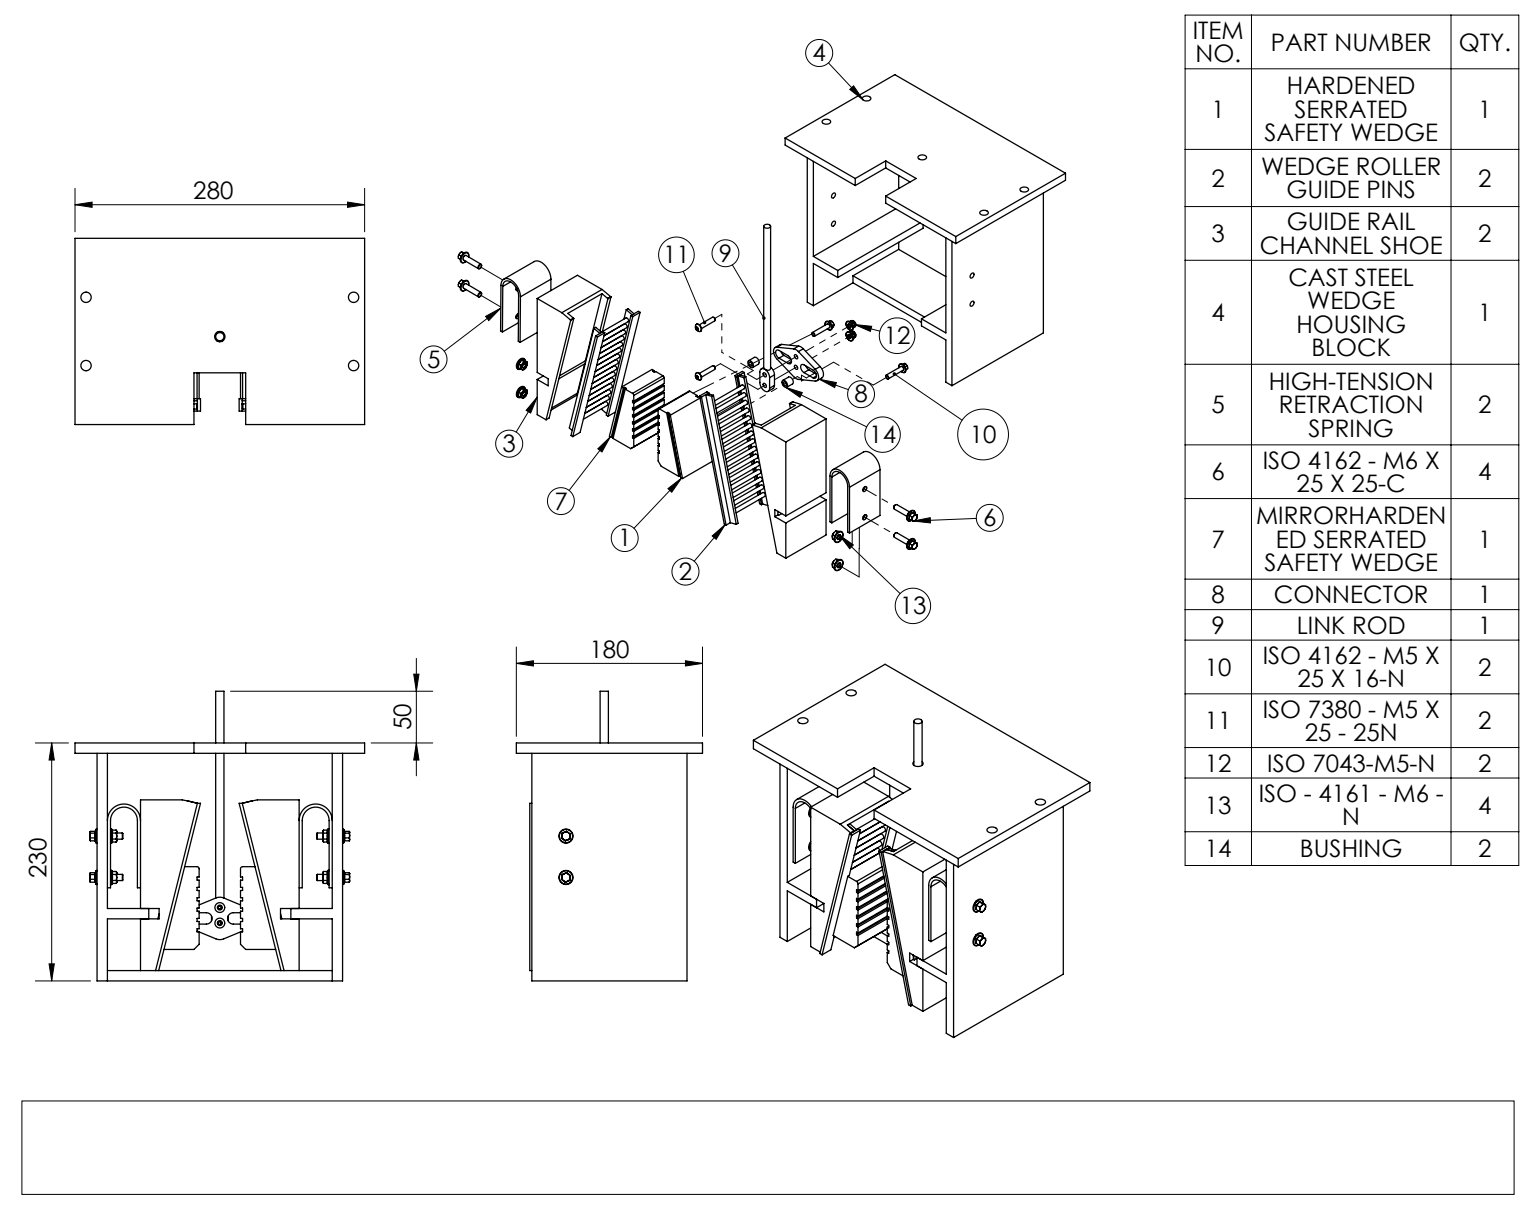
ISO-10303-21;
HEADER;
FILE_DESCRIPTION (('STEP AP214'),
    '1' );
FILE_NAME ('BR-599',
    '2026-09-24T10:26:00',
    ( '' ),
    ( '' ),
    'SwSTEP 2.0',
    'SolidWorks 2026',
    '' );
FILE_SCHEMA (( 'AUTOMOTIVE_DESIGN' ));
ENDSEC;

DATA;
#1 = VERTEX_POINT ( 'NONE', #3163 ) ;
#2 = DIRECTION ( 'NONE',  ( -1.000000000000000000, 0.000000000000000000, 0.000000000000000000 ) ) ;
#3 = CARTESIAN_POINT ( 'NONE',  ( 34.85300976710104948, 100.8957249956400375, 25.00000000000000000 ) ) ;
#4 = FACE_OUTER_BOUND ( 'NONE', #1590, .T. ) ;
#5 = CARTESIAN_POINT ( 'NONE',  ( -13.00000000000000533, 35.49999999999997158, 8.000000000000007105 ) ) ;
#6 = CIRCLE ( 'NONE', #8168, 300.0000000000001137 ) ;
#7 = CARTESIAN_POINT ( 'NONE',  ( 59.10657227073432551, 3.881474981106830313, 25.00000000000000000 ) ) ;
#8 = DIRECTION ( 'NONE',  ( 1.000000000000000000, 0.000000000000000000, 0.000000000000000000 ) ) ;
#9 = CARTESIAN_POINT ( 'NONE',  ( -4.101948962585905356, 2.368261337751086604, -3.381124513963614575 ) ) ;
#10 = ORIENTED_EDGE ( 'NONE', *, *, #2223, .T. ) ;
#11 = CARTESIAN_POINT ( 'NONE',  ( 36.99999999999999289, 80.00000000000000000, -25.00000000000000000 ) ) ;
#12 = DIRECTION ( 'NONE',  ( -1.000000000000000000, 0.000000000000000000, 0.000000000000000000 ) ) ;
#13 = DIRECTION ( 'NONE',  ( 0.000000000000000000, 4.440892098500621231E-16, 1.000000000000000000 ) ) ;
#14 = AXIS2_PLACEMENT_3D ( 'NONE', #9418, #3869, #11768 ) ;
#15 = VECTOR ( 'NONE', #13017, 1000.000000000000114 ) ;
#16 = LINE ( 'NONE', #8451, #3074 ) ;
#17 = EDGE_CURVE ( 'NONE', #13288, #10667, #2123, .T. ) ;
#18 = DIRECTION ( 'NONE',  ( 0.000000000000000000, -1.000000000000000000, 0.000000000000000000 ) ) ;
#19 = DIRECTION ( 'NONE',  ( -0.2425356250363330801, 0.9701425001453319874, 0.000000000000000000 ) ) ;
#20 = DIRECTION ( 'NONE',  ( -1.000000000000000000, 0.000000000000000000, 0.000000000000000000 ) ) ;
#21 = AXIS2_PLACEMENT_3D ( 'NONE', #11051, #3233, #13332 ) ;
#22 = CARTESIAN_POINT ( 'NONE',  ( 0.000000000000000000, 25.49999999999996803, 8.000000000000007105 ) ) ;
#23 = ORIENTED_EDGE ( 'NONE', *, *, #4123, .F. ) ;
#24 = COLOUR_RGB ( '', 0.66274510, 0.83137255, 0.94901961) ;
#25 = VERTEX_POINT ( 'NONE', #5412 ) ;
#26 = LINE ( 'NONE', #9828, #8340 ) ;
#27 = CONICAL_SURFACE ( 'NONE', #253, 2.540000000000002700, 0.7853981633974502774 ) ;
#28 = FILL_AREA_STYLE ('',( #13572 ) ) ;
#29 = VERTEX_POINT ( 'NONE', #870 ) ;
#30 = ADVANCED_FACE ( 'NONE', ( #11114 ), #7526, .T. ) ;
#31 = CARTESIAN_POINT ( 'NONE',  ( 0.1217565302851067177, -3.710888496608912845, 0.5725525826504656024 ) ) ;
#32 = VERTEX_POINT ( 'NONE', #2048 ) ;
#33 = ORIENTED_EDGE ( 'NONE', *, *, #5062, .T. ) ;
#34 = CONICAL_SURFACE ( 'NONE', #739, 4.000000000000004441, 1.047197551196600296 ) ;
#35 = VECTOR ( 'NONE', #3157, 1000.000000000000000 ) ;
#36 = VERTEX_POINT ( 'NONE', #7746 ) ;
#37 = EDGE_CURVE ( 'NONE', #1523, #9034, #1990, .T. ) ;
#38 = CARTESIAN_POINT ( 'NONE',  ( 3.903127820947815962E-15, 5.773502691896270633, -0.5999999999999894307 ) ) ;
#39 = LINE ( 'NONE', #7923, #9383 ) ;
#40 = CARTESIAN_POINT ( 'NONE',  ( 4.086376042167607636, -4.082715877136871008, 0.07147133206917684334 ) ) ;
#41 = CARTESIAN_POINT ( 'NONE',  ( -2.682243648011666259, -3.070208061305319536, -0.04852650426602220929 ) ) ;
#42 =( NAMED_UNIT ( * ) SI_UNIT ( $, .STERADIAN. ) SOLID_ANGLE_UNIT ( ) );
#43 = DIRECTION ( 'NONE',  ( 0.000000000000000000, 1.000000000000000000, 0.000000000000000000 ) ) ;
#44 = CARTESIAN_POINT ( 'NONE',  ( 4.050823680195247078, 3.779313952391380127, -0.5899027668435176119 ) ) ;
#45 = VERTEX_POINT ( 'NONE', #1089 ) ;
#46 = FILL_AREA_STYLE ('',( #8750 ) ) ;
#47 = VERTEX_POINT ( 'NONE', #6364 ) ;
#48 = AXIS2_PLACEMENT_3D ( 'NONE', #14299, #4291, #8725 ) ;
#49 = CARTESIAN_POINT ( 'NONE',  ( -129.3408537872145132, 199.5765550933606107, -75.00000000000001421 ) ) ;
#50 = CIRCLE ( 'NONE', #10087, 2.500000000000002220 ) ;
#51 = CIRCLE ( 'NONE', #7981, 2.500000000000002220 ) ;
#52 = DIRECTION ( 'NONE',  ( 0.000000000000000000, 0.000000000000000000, -1.000000000000000000 ) ) ;
#53 = EDGE_CURVE ( 'NONE', #1573, #2995, #7662, .T. ) ;
#54 = ORIENTED_EDGE ( 'NONE', *, *, #9609, .T. ) ;
#55 = VERTEX_POINT ( 'NONE', #5546 ) ;
#56 = ORIENTED_EDGE ( 'NONE', *, *, #8567, .F. ) ;
#57 = DIRECTION ( 'NONE',  ( 0.000000000000000000, 0.000000000000000000, -1.000000000000000000 ) ) ;
#58 = EDGE_CURVE ( 'NONE', #2255, #14288, #3932, .T. ) ;
#59 = MECHANICAL_DESIGN_GEOMETRIC_PRESENTATION_REPRESENTATION (  '', ( #3339 ), #8217 ) ;
#60 = ORIENTED_EDGE ( 'NONE', *, *, #8052, .T. ) ;
#61 = CARTESIAN_POINT ( 'NONE',  ( 0.000000000000000000, -0.8660254037844428154, 1.500000000000001332 ) ) ;
#62 = CIRCLE ( 'NONE', #4962, 5.000000000000000888 ) ;
#63 = PRODUCT ( 'bushing', 'bushing', '', ( #1978 ) ) ;
#64 = CARTESIAN_POINT ( 'NONE',  ( 0.000000000000000000, 0.000000000000000000, 0.000000000000000000 ) ) ;
#65 = CARTESIAN_POINT ( 'NONE',  ( 0.000000000000000000, 0.000000000000000000, -3.699999999999981082 ) ) ;
#66 = LINE ( 'NONE', #136, #7181 ) ;
#67 = B_SPLINE_CURVE_WITH_KNOTS ( 'NONE', 3,
 ( #11560, #3741, #1534, #5910, #10391, #8105 ),
 .UNSPECIFIED., .F., .F.,
 ( 4, 2, 4 ),
 ( 0.002365888236227980772, 0.003551327329835084114, 0.004736766423442187457 ),
 .UNSPECIFIED. ) ;
#68 = DIRECTION ( 'NONE',  ( -1.000000000000000000, 0.000000000000000000, 0.000000000000000000 ) ) ;
#69 = CARTESIAN_POINT ( 'NONE',  ( 22.00000000000000355, 30.00000000000000711, -25.00000000000000000 ) ) ;
#70 = LINE ( 'NONE', #7950, #11481 ) ;
#71 = MECHANICAL_DESIGN_GEOMETRIC_PRESENTATION_REPRESENTATION (  '', ( #7530 ), #1232 ) ;
#72 = EDGE_CURVE ( 'NONE', #4842, #5455, #11044, .T. ) ;
#73 = VERTEX_POINT ( 'NONE', #1987 ) ;
#74 = AXIS2_PLACEMENT_3D ( 'NONE', #8274, #12524, #8346 ) ;
#75 = EDGE_CURVE ( 'NONE', #7740, #14384, #13409, .T. ) ;
#76 = CARTESIAN_POINT ( 'NONE',  ( 4.142654963991838635, -2.035398498734361183, 3.525413613457314188 ) ) ;
#77 = AXIS2_PLACEMENT_3D ( 'NONE', #6500, #5341, #2338 ) ;
#78 = ORIENTED_EDGE ( 'NONE', *, *, #9945, .T. ) ;
#79 = VERTEX_POINT ( 'NONE', #5274 ) ;
#80 = CARTESIAN_POINT ( 'NONE',  ( 2.750000000000003997, 40.49999999999999289, 8.000000000000007105 ) ) ;
#81 = ORIENTED_EDGE ( 'NONE', *, *, #3321, .F. ) ;
#82 = CARTESIAN_POINT ( 'NONE',  ( -108.6817075744281595, 69.57655509336026967, 0.000000000000000000 ) ) ;
#83 = CARTESIAN_POINT ( 'NONE',  ( -5.000000000000000000, 0.9888715124523217437, -0.07061148569344526116 ) ) ;
#84 = CARTESIAN_POINT ( 'NONE',  ( -5.244935917792783897, 2.071347852254889155, -4.480280589322315876 ) ) ;
#85 = CARTESIAN_POINT ( 'NONE',  ( 2.855764796983339515, -2.970025579236438951, -0.09382832055446838071 ) ) ;
#86 = AXIS2_PLACEMENT_3D ( 'NONE', #5868, #6092, #4935 ) ;
#87 = EDGE_LOOP ( 'NONE', ( #13526, #11711, #10761, #2317 ) ) ;
#88 = FACE_OUTER_BOUND ( 'NONE', #2247, .T. ) ;
#89 = LINE ( 'NONE', #9889, #12206 ) ;
#90 = SURFACE_STYLE_FILL_AREA ( #4690 ) ;
#91 = DIRECTION ( 'NONE',  ( -0.000000000000000000, -0.000000000000000000, -1.000000000000000000 ) ) ;
#92 = ORIENTED_EDGE ( 'NONE', *, *, #1429, .T. ) ;
#93 = AXIS2_PLACEMENT_3D ( 'NONE', #10441, #13974, #10675 ) ;
#94 = CARTESIAN_POINT ( 'NONE',  ( -2.000000000000003997, 3.464101615137761492, -2.842992957459211212 ) ) ;
#95 = ADVANCED_FACE ( 'NONE', ( #9801 ), #3380, .T. ) ;
#96 = ADVANCED_FACE ( 'NONE', ( #3591 ), #13623, .F. ) ;
#97 = LINE ( 'NONE', #11278, #533 ) ;
#98 = DIRECTION ( 'NONE',  ( 0.000000000000000000, -1.000000000000000000, 0.000000000000000000 ) ) ;
#99 = PRODUCT_DEFINITION_SHAPE ( 'NONE', 'NONE',  #14480 ) ;
#100 = ORIENTED_EDGE ( 'NONE', *, *, #751, .T. ) ;
#101 = DIRECTION ( 'NONE',  ( 0.000000000000000000, 0.000000000000000000, -1.000000000000000000 ) ) ;
#102 = LINE ( 'NONE', #4701, #4263 ) ;
#103 = CARTESIAN_POINT ( 'NONE',  ( 0.000000000000000000, 0.000000000000000000, 1.599999999999990319 ) ) ;
#104 = CARTESIAN_POINT ( 'NONE',  ( 4.942471129496375681, -1.621204395475712046, 4.000000000000003553 ) ) ;
#105 = ORIENTED_EDGE ( 'NONE', *, *, #7029, .T. ) ;
#106 = LINE ( 'NONE', #11351, #1126 ) ;
#107 = EDGE_CURVE ( 'NONE', #8048, #4572, #11469, .T. ) ;
#108 =( NAMED_UNIT ( * ) PLANE_ANGLE_UNIT ( ) SI_UNIT ( $, .RADIAN. ) );
#109 = EDGE_CURVE ( 'NONE', #144, #5025, #8095, .T. ) ;
#110 = ORIENTED_EDGE ( 'NONE', *, *, #1310, .T. ) ;
#111 = CARTESIAN_POINT ( 'NONE',  ( 5.551115123125782702E-14, 3.464101615137764156, 2.000000000000001776 ) ) ;
#112 = ORIENTED_EDGE ( 'NONE', *, *, #12518, .T. ) ;
#113 = DIRECTION ( 'NONE',  ( 1.000000000000000000, 0.000000000000000000, -0.000000000000000000 ) ) ;
#114 = CYLINDRICAL_SURFACE ( 'NONE', #8701, 2.500000000000002220 ) ;
#115 = LINE ( 'NONE', #14321, #13122 ) ;
#116 = DIRECTION ( 'NONE',  ( 1.000000000000000000, 0.000000000000000000, 0.000000000000000000 ) ) ;
#117 = DIRECTION ( 'NONE',  ( -2.273843122241288438E-18, -5.551115123125783935E-17, -1.000000000000000000 ) ) ;
#118 = EDGE_CURVE ( 'NONE', #4637, #7467, #9051, .T. ) ;
#119 = CARTESIAN_POINT ( 'NONE',  ( 4.071447262713911996, -2.020725942163681399, 3.499999999999989342 ) ) ;
#120 = CARTESIAN_POINT ( 'NONE',  ( 22.00000000000000355, 30.00000000000000711, -25.00000000000000000 ) ) ;
#121 = ORIENTED_EDGE ( 'NONE', *, *, #9321, .T. ) ;
#122 = DIRECTION ( 'NONE',  ( -0.000000000000000000, -1.000000000000000000, -0.000000000000000000 ) ) ;
#123 = ADVANCED_FACE ( 'NONE', ( #3728 ), #1486, .F. ) ;
#124 = DIRECTION ( 'NONE',  ( -1.000000000000000000, -1.224646799147353454E-16, 0.000000000000000000 ) ) ;
#125 = EDGE_CURVE ( 'NONE', #5215, #588, #8984, .T. ) ;
#126 = ORIENTED_EDGE ( 'NONE', *, *, #8617, .F. ) ;
#127 = ORIENTED_EDGE ( 'NONE', *, *, #5175, .F. ) ;
#128 = ORIENTED_EDGE ( 'NONE', *, *, #2234, .F. ) ;
#129 = FACE_OUTER_BOUND ( 'NONE', #6696, .T. ) ;
#130 = EDGE_CURVE ( 'NONE', #3893, #6812, #6927, .T. ) ;
#131 = VERTEX_POINT ( 'NONE', #10090 ) ;
#132 = DIRECTION ( 'NONE',  ( -1.000000000000000000, -3.286707217423839940E-17, -2.273843122241288053E-18 ) ) ;
#133 = DIRECTION ( 'NONE',  ( -1.000000000000000000, 2.551526159633733968E-19, 1.987661601597216239E-18 ) ) ;
#134 = DIRECTION ( 'NONE',  ( 0.000000000000000000, 0.000000000000000000, 1.000000000000000000 ) ) ;
#135 = ADVANCED_FACE ( 'NONE', ( #12436 ), #6529, .F. ) ;
#136 = CARTESIAN_POINT ( 'NONE',  ( 19.99999999999999645, 67.00000000000000000, -25.00000000000000000 ) ) ;
#137 = CARTESIAN_POINT ( 'NONE',  ( 3.000000000000000888, 3.469446951953614189E-15, -25.03750572909319061 ) ) ;
#138 = AXIS2_PLACEMENT_3D ( 'NONE', #9240, #11510, #4853 ) ;
#139 = FACE_OUTER_BOUND ( 'NONE', #10085, .T. ) ;
#140 = DIRECTION ( 'NONE',  ( 0.000000000000000000, 1.000000000000000000, 0.000000000000000000 ) ) ;
#141 = EDGE_CURVE ( 'NONE', #4176, #9400, #11330, .T. ) ;
#142 = CARTESIAN_POINT ( 'NONE',  ( 5.085009042717538286, 2.271170964606955778, 4.066216496625539634 ) ) ;
#143 = ORIENTED_EDGE ( 'NONE', *, *, #10591, .T. ) ;
#144 = VERTEX_POINT ( 'NONE', #80 ) ;
#145 = CARTESIAN_POINT ( 'NONE',  ( -2.712778981739159878, 3.052578478157618846, -3.130620751972420734 ) ) ;
#146 = ORIENTED_EDGE ( 'NONE', *, *, #7792, .F. ) ;
#147 = EDGE_LOOP ( 'NONE', ( #10800, #705, #1394, #14407 ) ) ;
#148 = CARTESIAN_POINT ( 'NONE',  ( 0.8653900595644522520, -5.556556492855608376, -4.490801088233122407 ) ) ;
#149 = LINE ( 'NONE', #2412, #13592 ) ;
#150 = EDGE_CURVE ( 'NONE', #7089, #2949, #9184, .T. ) ;
#151 = CARTESIAN_POINT ( 'NONE',  ( 2.171643655288374664, -3.365003104552342972, -1.643201566025979943E-14 ) ) ;
#152 = CARTESIAN_POINT ( 'NONE',  ( 6.800000000000028244, -4.618802153517003184, 0.000000000000000000 ) ) ;
#153 = FACE_OUTER_BOUND ( 'NONE', #11102, .T. ) ;
#154 = CARTESIAN_POINT ( 'NONE',  ( 58.68170757442803165, 29.57655509336062849, -33.00000000000000000 ) ) ;
#155 = ORIENTED_EDGE ( 'NONE', *, *, #6137, .F. ) ;
#156 = CARTESIAN_POINT ( 'NONE',  ( 0.2484800633749933707, -4.430380094434230642, -0.3263565795981031581 ) ) ;
#157 = AXIS2_PLACEMENT_3D ( 'NONE', #14374, #7610, #12245 ) ;
#158 = ORIENTED_EDGE ( 'NONE', *, *, #2244, .F. ) ;
#159 = CARTESIAN_POINT ( 'NONE',  ( 56.68121602037099649, 13.58289998256015352, 25.00000000000000000 ) ) ;
#160 = LINE ( 'NONE', #229, #1194 ) ;
#161 = EDGE_CURVE ( 'NONE', #1060, #1016, #5743, .T. ) ;
#162 = DIRECTION ( 'NONE',  ( 0.000000000000000000, -1.000000000000000000, 0.000000000000000000 ) ) ;
#163 = EDGE_CURVE ( 'NONE', #6145, #1954, #4682, .T. ) ;
#164 = ORIENTED_EDGE ( 'NONE', *, *, #6756, .F. ) ;
#165 = DIRECTION ( 'NONE',  ( 1.734723475976770502E-18, -4.440892098500621231E-16, -1.000000000000000000 ) ) ;
#166 = VECTOR ( 'NONE', #2081, 1000.000000000000000 ) ;
#167 = CARTESIAN_POINT ( 'NONE',  ( 0.000000000000000000, 0.000000000000000000, 0.000000000000000000 ) ) ;
#168 = CONICAL_SURFACE ( 'NONE', #12822, 1732.050807568857181, 1.047197551196592746 ) ;
#169 = ORIENTED_EDGE ( 'NONE', *, *, #8329, .T. ) ;
#170 = CARTESIAN_POINT ( 'NONE',  ( 59.91362529070399034, 29.57655509336063560, -28.00000000000000000 ) ) ;
#171 = PRODUCT_DEFINITION_SHAPE ( 'NONE', 'NONE',  #7761 ) ;
#172 = VERTEX_POINT ( 'NONE', #3659 ) ;
#173 = FACE_OUTER_BOUND ( 'NONE', #6648, .T. ) ;
#174 = LINE ( 'NONE', #1203, #523 ) ;
#175 = AXIS2_PLACEMENT_3D ( 'NONE', #2230, #7697, #10922 ) ;
#176 = AXIS2_PLACEMENT_3D ( 'NONE', #8540, #7429, #5033 ) ;
#177 = DIRECTION ( 'NONE',  ( 0.000000000000000000, 0.000000000000000000, -1.000000000000000000 ) ) ;
#178 = LINE ( 'NONE', #1338, #11397 ) ;
#179 =( NAMED_UNIT ( * ) PLANE_ANGLE_UNIT ( ) SI_UNIT ( $, .RADIAN. ) );
#180 = LINE ( 'NONE', #12266, #3484 ) ;
#181 = VERTEX_POINT ( 'NONE', #10380 ) ;
#182 = CARTESIAN_POINT ( 'NONE',  ( 0.000000000000000000, 0.000000000000000000, 0.000000000000000000 ) ) ;
#183 = ORIENTED_EDGE ( 'NONE', *, *, #4806, .T. ) ;
#184 = DIRECTION ( 'NONE',  ( -1.000000000000000000, 0.000000000000000000, 0.000000000000000000 ) ) ;
#185 = ORIENTED_EDGE ( 'NONE', *, *, #3525, .T. ) ;
#186 = DIRECTION ( 'NONE',  ( 0.000000000000000000, 0.000000000000000000, -1.000000000000000000 ) ) ;
#187 = AXIS2_PLACEMENT_3D ( 'NONE', #14289, #6433, #6375 ) ;
#188 = AXIS2_PLACEMENT_3D ( 'NONE', #12778, #9636, #495 ) ;
#189 = EDGE_LOOP ( 'NONE', ( #816, #9707, #13523, #12144 ) ) ;
#190 = EDGE_LOOP ( 'NONE', ( #12989, #13833, #3490, #10771 ) ) ;
#191 = FACE_OUTER_BOUND ( 'NONE', #2606, .T. ) ;
#192 = VERTEX_POINT ( 'NONE', #361 ) ;
#193 = PLANE ( 'NONE',  #1641 ) ;
#194 = EDGE_CURVE ( 'NONE', #2847, #8895, #12600, .T. ) ;
#195 = ADVANCED_FACE ( 'NONE', ( #8392 ), #5103, .F. ) ;
#196 = AXIS2_PLACEMENT_3D ( 'NONE', #5459, #4385, #14329 ) ;
#197 = DIRECTION ( 'NONE',  ( -1.000000000000000000, -0.000000000000000000, -0.000000000000000000 ) ) ;
#198 = LINE ( 'NONE', #5806, #5338 ) ;
#199 = VECTOR ( 'NONE', #5956, 1000.000000000000000 ) ;
#200 = ITEM_DEFINED_TRANSFORMATION ( 'NONE', 'NONE', #5460,  #11025 ) ;
#201 = VECTOR ( 'NONE', #12349, 1000.000000000000000 ) ;
#202 = PLANE ( 'NONE',  #7722 ) ;
#203 = CARTESIAN_POINT ( 'NONE',  ( -4.204114099329524734, 1.660341531092956124, -3.302132361967865748 ) ) ;
#204 = CARTESIAN_POINT ( 'NONE',  ( 4.071447262713911996, 2.020725942163681399, -3.499999999999996003 ) ) ;
#205 = EDGE_CURVE ( 'NONE', #13026, #14419, #660, .T. ) ;
#206 = EDGE_CURVE ( 'NONE', #7155, #8446, #11531, .T. ) ;
#207 = ORIENTED_EDGE ( 'NONE', *, *, #6472, .T. ) ;
#208 = AXIS2_PLACEMENT_3D ( 'NONE', #12173, #7777, #14450 ) ;
#209 = ORIENTED_EDGE ( 'NONE', *, *, #6776, .T. ) ;
#210 = CARTESIAN_POINT ( 'NONE',  ( 22.00000000000000355, 40.00000000000000711, 25.00000000000000000 ) ) ;
#211 = ORIENTED_EDGE ( 'NONE', *, *, #12673, .T. ) ;
#212 = DIRECTION ( 'NONE',  ( 0.000000000000000000, 1.000000000000000000, 0.000000000000000000 ) ) ;
#213 = EDGE_CURVE ( 'NONE', #6553, #4911, #14362, .T. ) ;
#214 = CARTESIAN_POINT ( 'NONE',  ( 8.000000000000000000, 25.49999999999996803, 8.000000000000007105 ) ) ;
#215 = LINE ( 'NONE', #3596, #1161 ) ;
#216 = CARTESIAN_POINT ( 'NONE',  ( 0.1391502195351374815, -4.241015250120806712, 0.6543461111163237920 ) ) ;
#217 = CARTESIAN_POINT ( 'NONE',  ( 56.75585977000769589, 23.28432498401347672, 25.00000000000000000 ) ) ;
#218 = DIRECTION ( 'NONE',  ( 0.000000000000000000, 0.000000000000000000, 1.000000000000000000 ) ) ;
#219 = CARTESIAN_POINT ( 'NONE',  ( 62.10586122665984732, -20.42344490663941414, -23.00000000000000000 ) ) ;
#220 = EDGE_LOOP ( 'NONE', ( #2917, #1884 ) ) ;
#221 = AXIS2_PLACEMENT_3D ( 'NONE', #6634, #1226, #3433 ) ;
#222 = DIRECTION ( 'NONE',  ( 1.000000000000000000, 0.000000000000000000, 0.000000000000000000 ) ) ;
#223 = VECTOR ( 'NONE', #6277, 1000.000000000000000 ) ;
#224 = ORIENTED_EDGE ( 'NONE', *, *, #11005, .F. ) ;
#225 = EDGE_CURVE ( 'NONE', #10568, #2459, #4887, .T. ) ;
#226 = ORIENTED_EDGE ( 'NONE', *, *, #6230, .T. ) ;
#227 = AXIS2_PLACEMENT_3D ( 'NONE', #3286, #6852, #12205 ) ;
#228 = CARTESIAN_POINT ( 'NONE',  ( 22.00000000000000000, 67.00000000000000000, 25.00000000000000000 ) ) ;
#229 = CARTESIAN_POINT ( 'NONE',  ( 24.99999999999999289, -4.898587196589414604E-15, -25.00000000000000000 ) ) ;
#230 = EDGE_CURVE ( 'NONE', #2483, #11506, #8245, .T. ) ;
#231 = FILL_AREA_STYLE_COLOUR ( '', #8450 ) ;
#232 = B_SPLINE_CURVE_WITH_KNOTS ( 'NONE', 3,
 ( #9885, #3384, #13193, #4342, #3307, #6720, #12149, #7750, #12227, #4273 ),
 .UNSPECIFIED., .F., .F.,
 ( 4, 2, 2, 2, 4 ),
 ( 0.000000000000000000, 0.001528561485809837566, 0.003057122971619675132, 0.004585684457429512265, 0.006114245943239350264 ),
 .UNSPECIFIED. ) ;
#233 = ORIENTED_EDGE ( 'NONE', *, *, #8707, .F. ) ;
#234 = ORIENTED_EDGE ( 'NONE', *, *, #1565, .T. ) ;
#235 = CARTESIAN_POINT ( 'NONE',  ( 0.000000000000000000, 25.49999999999996803, 8.000000000000007105 ) ) ;
#236 = DIRECTION ( 'NONE',  ( 1.000000000000000000, -0.000000000000000000, -0.000000000000000000 ) ) ;
#237 = AXIS2_PLACEMENT_3D ( 'NONE', #9091, #4649, #3762 ) ;
#238 = ORIENTED_EDGE ( 'NONE', *, *, #350, .F. ) ;
#239 = EDGE_CURVE ( 'NONE', #9259, #13438, #9577, .T. ) ;
#240 = CARTESIAN_POINT ( 'NONE',  ( -5.184911785341042467, -2.993510214990505514, -4.630720594357042863 ) ) ;
#241 = EDGE_CURVE ( 'NONE', #3192, #10542, #6150, .T. ) ;
#242 = CARTESIAN_POINT ( 'NONE',  ( 4.000000000000003553, 2.309401076758501592, -4.699999999999981526 ) ) ;
#243 = DIRECTION ( 'NONE',  ( 1.000000000000000000, 1.723842398015259277E-15, 0.000000000000000000 ) ) ;
#244 = B_SPLINE_CURVE_WITH_KNOTS ( 'NONE', 3,
 ( #6085, #473, #399, #10567, #328 ),
 .UNSPECIFIED., .F., .F.,
 ( 4, 1, 4 ),
 ( 0.000000000000000000, 0.002309401076758502321, 0.004618802153517004641 ),
 .UNSPECIFIED. ) ;
#245 = ORIENTED_EDGE ( 'NONE', *, *, #3357, .T. ) ;
#246 = AXIS2_PLACEMENT_3D ( 'NONE', #2195, #9875, #11107 ) ;
#247 = CARTESIAN_POINT ( 'NONE',  ( 4.175326769692832229, -2.060699556488890138, -3.569236330973504678 ) ) ;
#248 = CIRCLE ( 'NONE', #2365, 2.500000000000000444 ) ;
#249 = DIRECTION ( 'NONE',  ( 1.000000000000000000, -2.551526159633733968E-19, -1.987661601597216239E-18 ) ) ;
#250 = PRESENTATION_STYLE_ASSIGNMENT (( #7854 ) ) ;
#251 = DIRECTION ( 'NONE',  ( 2.732679788978641511E-17, 0.8660254037844375974, -0.5000000000000019984 ) ) ;
#252 = LINE ( 'NONE', #13664, #5773 ) ;
#253 = AXIS2_PLACEMENT_3D ( 'NONE', #8429, #2964, #14156 ) ;
#254 = VERTEX_POINT ( 'NONE', #10524 ) ;
#255 = DIRECTION ( 'NONE',  ( 0.000000000000000000, 0.000000000000000000, 1.000000000000000000 ) ) ;
#256 = ORIENTED_EDGE ( 'NONE', *, *, #409, .F. ) ;
#257 = FACE_OUTER_BOUND ( 'NONE', #7644, .T. ) ;
#258 = VECTOR ( 'NONE', #7960, 1000.000000000000000 ) ;
#259 = FACE_OUTER_BOUND ( 'NONE', #5577, .T. ) ;
#260 = VERTEX_POINT ( 'NONE', #11845 ) ;
#261 = LINE ( 'NONE', #9100, #14213 ) ;
#262 = VECTOR ( 'NONE', #2943, 1000.000000000000114 ) ;
#263 = AXIS2_PLACEMENT_3D ( 'NONE', #12477, #3770, #2452 ) ;
#264 = ADVANCED_FACE ( 'NONE', ( #14056 ), #3951, .T. ) ;
#265 = EDGE_LOOP ( 'NONE', ( #8330, #2797, #508, #8925 ) ) ;
#266 = ORIENTED_EDGE ( 'NONE', *, *, #8071, .F. ) ;
#267 = ORIENTED_EDGE ( 'NONE', *, *, #8811, .F. ) ;
#268 = CIRCLE ( 'NONE', #9369, 5.000000000000004441 ) ;
#269 = VERTEX_POINT ( 'NONE', #12870 ) ;
#270 = DIRECTION ( 'NONE',  ( 0.000000000000000000, -8.482162385747133845E-47, 1.000000000000000000 ) ) ;
#271 = CARTESIAN_POINT ( 'NONE',  ( 66.53192852109765454, -5.819950020346492892, -25.00000000000000000 ) ) ;
#272 = ORIENTED_EDGE ( 'NONE', *, *, #3606, .T. ) ;
#273 = FACE_OUTER_BOUND ( 'NONE', #4402, .T. ) ;
#274 = CARTESIAN_POINT ( 'NONE',  ( 5.253687138749954855, 3.069401043531180484, -4.666239469495483405 ) ) ;
#275 = FILL_AREA_STYLE_COLOUR ( '', #447 ) ;
#276 = DIRECTION ( 'NONE',  ( 0.000000000000000000, 0.000000000000000000, 1.000000000000000000 ) ) ;
#277 = PRESENTATION_LAYER_ASSIGNMENT (  '', '', ( #3555 ) ) ;
#278 = VECTOR ( 'NONE', #5827, 1000.000000000000227 ) ;
#279 = CARTESIAN_POINT ( 'NONE',  ( 0.2174200650117580069, 3.876582599186215727, 0.2855619784720741516 ) ) ;
#280 = CYLINDRICAL_SURFACE ( 'NONE', #1408, 2.500000000000002220 ) ;
#281 = FACE_OUTER_BOUND ( 'NONE', #2970, .T. ) ;
#282 = CARTESIAN_POINT ( 'NONE',  ( 5.000000000000001776, -0.9835753746177059442, -0.05800540215398873600 ) ) ;
#283 = EDGE_CURVE ( 'NONE', #3285, #4147, #432, .T. ) ;
#284 = VECTOR ( 'NONE', #9089, 1000.000000000000000 ) ;
#285 = COLOUR_RGB ( '', 0.40784314, 0.44705882, 0.49803922) ;
#286 = ORIENTED_EDGE ( 'NONE', *, *, #14219, .T. ) ;
#287 = AXIS2_PLACEMENT_3D ( 'NONE', #9499, #13966, #10597 ) ;
#288 = VECTOR ( 'NONE', #14234, 1000.000000000000000 ) ;
#289 = ORIENTED_EDGE ( 'NONE', *, *, #2632, .T. ) ;
#290 = DIRECTION ( 'NONE',  ( -1.000000000000000000, 0.000000000000000000, 0.000000000000000000 ) ) ;
#291 = ORIENTED_EDGE ( 'NONE', *, *, #5105, .F. ) ;
#292 = ORIENTED_EDGE ( 'NONE', *, *, #11801, .F. ) ;
#293 = EDGE_CURVE ( 'NONE', #3067, #10101, #2628, .T. ) ;
#294 = FACE_OUTER_BOUND ( 'NONE', #7069, .T. ) ;
#295 = DIRECTION ( 'NONE',  ( -1.000000000000000000, -1.665334536937734318E-16, 0.000000000000000000 ) ) ;
#296 = CARTESIAN_POINT ( 'NONE',  ( 61.53192852109764743, -5.819950020346492892, -25.00000000000000000 ) ) ;
#297 = CARTESIAN_POINT ( 'NONE',  ( 28.00000000000000355, 29.99999999999999645, -6.999999999999992006 ) ) ;
#298 = PLANE ( 'NONE',  #9372 ) ;
#299 = EDGE_CURVE ( 'NONE', #11445, #8749, #1752, .T. ) ;
#300 = DIRECTION ( 'NONE',  ( -1.000000000000000000, -1.276920294826118092E-16, 0.000000000000000000 ) ) ;
#301 = VECTOR ( 'NONE', #2565, 1000.000000000000000 ) ;
#302 = AXIS2_PLACEMENT_3D ( 'NONE', #9953, #7666, #5414 ) ;
#303 = PRODUCT_DEFINITION_SHAPE ( 'NONE', 'NONE',  #14478 ) ;
#304 = CARTESIAN_POINT ( 'NONE',  ( 63.34848382498275754, 15.83712095624566984, 0.000000000000000000 ) ) ;
#305 = EDGE_CURVE ( 'NONE', #1178, #14168, #3877, .T. ) ;
#306 = EDGE_LOOP ( 'NONE', ( #9617, #6629, #11279, #5233, #2336 ) ) ;
#307 = UNCERTAINTY_MEASURE_WITH_UNIT (LENGTH_MEASURE( 1.000000000000000082E-05 ), #6803, 'distance_accuracy_value', 'NONE');
#308 = AXIS2_PLACEMENT_3D ( 'NONE', #4405, #11111, #14418 ) ;
#309 = CARTESIAN_POINT ( 'NONE',  ( -4.177163563997808592E-15, -5.914770570062451327, -4.581776566113613391 ) ) ;
#310 = DIRECTION ( 'NONE',  ( -0.000000000000000000, -0.000000000000000000, -1.000000000000000000 ) ) ;
#311 = EDGE_CURVE ( 'NONE', #7235, #651, #5038, .T. ) ;
#312 = EDGE_CURVE ( 'NONE', #10181, #36, #9348, .T. ) ;
#313 = VERTEX_POINT ( 'NONE', #3807 ) ;
#314 = LINE ( 'NONE', #11495, #3240 ) ;
#315 = AXIS2_PLACEMENT_3D ( 'NONE', #13880, #3856, #13947 ) ;
#316 = CARTESIAN_POINT ( 'NONE',  ( 5.000882498481321825, 2.309401076758504257, -4.000000000000005329 ) ) ;
#317 = ORIENTED_EDGE ( 'NONE', *, *, #8785, .T. ) ;
#318 = DIRECTION ( 'NONE',  ( 0.000000000000000000, 0.000000000000000000, -1.000000000000000000 ) ) ;
#319 = AXIS2_PLACEMENT_3D ( 'NONE', #14262, #4250, #9862 ) ;
#320 = ORIENTED_EDGE ( 'NONE', *, *, #6806, .T. ) ;
#321 = CARTESIAN_POINT ( 'NONE',  ( -1.655952806101420816, 3.662737355149043417, -7.859618717572649691E-15 ) ) ;
#322 = CARTESIAN_POINT ( 'NONE',  ( 4.960798468789974436, -4.316040323963732384, 0.6738506825564457570 ) ) ;
#323 = CARTESIAN_POINT ( 'NONE',  ( 4.142654963991838635, -2.035398498734360739, -3.525413613457307083 ) ) ;
#324 = PLANE ( 'NONE',  #4421 ) ;
#325 = FILL_AREA_STYLE ('',( #4788 ) ) ;
#326 = CARTESIAN_POINT ( 'NONE',  ( 5.211749180171795892, 2.764497899775253398, -4.327903350935040194 ) ) ;
#327 = EDGE_CURVE ( 'NONE', #12296, #10667, #14351, .T. ) ;
#328 = CARTESIAN_POINT ( 'NONE',  ( 4.988724804725785944, -2.309401076758511806, -3.999999999999989786 ) ) ;
#329 = ORIENTED_EDGE ( 'NONE', *, *, #2055, .F. ) ;
#330 = FACE_OUTER_BOUND ( 'NONE', #10664, .T. ) ;
#331 = AXIS2_PLACEMENT_3D ( 'NONE', #13223, #14112, #7625 ) ;
#332 = EDGE_LOOP ( 'NONE', ( #2235, #9839 ) ) ;
#333 = CARTESIAN_POINT ( 'NONE',  ( 108.6817075744280174, -30.42344490663958112, 33.00000000000002842 ) ) ;
#334 = LINE ( 'NONE', #480, #12683 ) ;
#335 = ORIENTED_EDGE ( 'NONE', *, *, #3874, .F. ) ;
#336 = LINE ( 'NONE', #6016, #9990 ) ;
#337 = VERTEX_POINT ( 'NONE', #12933 ) ;
#338 = ORIENTED_EDGE ( 'NONE', *, *, #3386, .T. ) ;
#339 = DIRECTION ( 'NONE',  ( 1.000000000000000000, 0.000000000000000000, -0.000000000000000000 ) ) ;
#340 = EDGE_LOOP ( 'NONE', ( #2490, #1652, #2077 ) ) ;
#341 = CARTESIAN_POINT ( 'NONE',  ( 7.500000000000029310, 29.99999999999999289, 0.000000000000000000 ) ) ;
#342 = CYLINDRICAL_SURFACE ( 'NONE', #2622, 4.000000000000001776 ) ;
#343 = CLOSED_SHELL ( 'NONE', ( #348, #10277, #10610, #2946, #4930, #5603, #8583, #3122, #8964, #584, #2814, #2804, #5042, #11746, #8231, #7567, #9589, #9255, #10929, #2822, #4189, #8522, #2178, #12387, #5966, #9430, #5583, #8276, #5909 ) ) ;
#344 = ORIENTED_EDGE ( 'NONE', *, *, #679, .T. ) ;
#345 = DIRECTION ( 'NONE',  ( 0.000000000000000000, 0.000000000000000000, -1.000000000000000000 ) ) ;
#346 = CARTESIAN_POINT ( 'NONE',  ( 0.2484800633750008092, -2.497823135841239939, 3.673643420401929482 ) ) ;
#347 = PRESENTATION_STYLE_ASSIGNMENT (( #11533 ) ) ;
#348 = ADVANCED_FACE ( 'NONE', ( #1821 ), #11776, .T. ) ;
#349 = CARTESIAN_POINT ( 'NONE',  ( 5.599999999999994316, -4.041451884327377009, 0.000000000000000000 ) ) ;
#350 = EDGE_CURVE ( 'NONE', #1315, #10506, #376, .T. ) ;
#351 = DIRECTION ( 'NONE',  ( 0.000000000000000000, 0.000000000000000000, 1.000000000000000000 ) ) ;
#352 = CARTESIAN_POINT ( 'NONE',  ( 25.00000000000000000, 189.5765550933606107, 47.99999999999998579 ) ) ;
#353 = PLANE ( 'NONE',  #1336 ) ;
#354 = CARTESIAN_POINT ( 'NONE',  ( -2.749999999999997780, 25.49999999999996803, 8.000000000000007105 ) ) ;
#355 = CARTESIAN_POINT ( 'NONE',  ( 20.00000000000000000, 70.00000000000000000, 25.00000000000000000 ) ) ;
#356 = EDGE_CURVE ( 'NONE', #7502, #4025, #7084, .T. ) ;
#357 = ORIENTED_EDGE ( 'NONE', *, *, #6598, .T. ) ;
#358 = ORIENTED_EDGE ( 'NONE', *, *, #8649, .F. ) ;
#359 = EDGE_LOOP ( 'NONE', ( #6846, #13028, #8516, #4534 ) ) ;
#360 = AXIS2_PLACEMENT_3D ( 'NONE', #1411, #10345, #9164 ) ;
#361 = CARTESIAN_POINT ( 'NONE',  ( 35.00229726637439143, 120.2985749985466839, 25.00000000000000000 ) ) ;
#362 = ORIENTED_EDGE ( 'NONE', *, *, #4420, .T. ) ;
#363 = FACE_BOUND ( 'NONE', #5930, .T. ) ;
#364 = CARTESIAN_POINT ( 'NONE',  ( 5.122341571230623281, 2.957385285031203459, -4.581776566113601845 ) ) ;
#365 = CARTESIAN_POINT ( 'NONE',  ( 129.3408537872138595, 189.5765550933606107, -4.000000000000019540 ) ) ;
#366 = DIRECTION ( 'NONE',  ( 0.000000000000000000, 0.000000000000000000, 1.000000000000000000 ) ) ;
#367 = EDGE_CURVE ( 'NONE', #6880, #5464, #10123, .T. ) ;
#368 = CARTESIAN_POINT ( 'NONE',  ( 1.671902908347949033E-15, 2.686816014504571193, 2.346298152288376127 ) ) ;
#369 = DIRECTION ( 'NONE',  ( 1.000000000000000000, 0.000000000000000000, 0.000000000000000000 ) ) ;
#370 = ADVANCED_FACE ( 'NONE', ( #3209 ), #923, .F. ) ;
#371 = LINE ( 'NONE', #6940, #6098 ) ;
#372 = DIRECTION ( 'NONE',  ( -1.000000000000000000, 0.000000000000000000, 0.000000000000000000 ) ) ;
#373 = VERTEX_POINT ( 'NONE', #7643 ) ;
#374 = AXIS2_PLACEMENT_3D ( 'NONE', #6234, #5287, #14092 ) ;
#375 = VERTEX_POINT ( 'NONE', #14335 ) ;
#376 = B_SPLINE_CURVE_WITH_KNOTS ( 'NONE', 3,
 ( #7503, #2032, #11022, #6628, #11096, #11995 ),
 .UNSPECIFIED., .F., .F.,
 ( 4, 2, 4 ),
 ( 0.01308430721348208085, 0.01410661710602280003, 0.01512892699856351920 ),
 .UNSPECIFIED. ) ;
#377 = ADVANCED_FACE ( 'NONE', ( #4324 ), #12061, .F. ) ;
#378 = ORIENTED_EDGE ( 'NONE', *, *, #1938, .F. ) ;
#379 = CARTESIAN_POINT ( 'NONE',  ( 4.851472949720997185, 2.694301256218259777, -3.333333333333333925 ) ) ;
#380 = DIRECTION ( 'NONE',  ( 0.000000000000000000, 0.000000000000000000, -1.000000000000000000 ) ) ;
#381 = EDGE_CURVE ( 'NONE', #10071, #10068, #6343, .T. ) ;
#382 = EDGE_CURVE ( 'NONE', #1594, #11544, #7791, .T. ) ;
#383 = ORIENTED_EDGE ( 'NONE', *, *, #7969, .F. ) ;
#384 = EDGE_LOOP ( 'NONE', ( #8379, #6792, #7299, #1071, #1051 ) ) ;
#385 = CARTESIAN_POINT ( 'NONE',  ( 54.33050351964436686, 32.98574998546678927, 25.00000000000000000 ) ) ;
#386 = CARTESIAN_POINT ( 'NONE',  ( 5.076540720129295359, 2.330508241952946147, -4.036558682520523966 ) ) ;
#387 = ORIENTED_EDGE ( 'NONE', *, *, #10769, .T. ) ;
#388 =( BOUNDED_SURFACE ( )  B_SPLINE_SURFACE ( 3, 2, ( 
 ( #3636, #8070, #4659 ),
 ( #3858, #7047, #7120 ),
 ( #6973, #4862, #11444 ),
 ( #3572, #2599, #9324 ),
 ( #12766, #9250, #13809 ),
 ( #13596, #1568, #3776 ) ),
 .UNSPECIFIED., .F., .F., .T. ) 
 B_SPLINE_SURFACE_WITH_KNOTS ( ( 4, 2, 4 ),
 ( 3, 3 ),
 ( 0.01886032586153034776, 0.02121253401777977582, 0.02356474217402920734 ),
 ( 0.000000000000000000, 1.000000000000000000 ),
 .UNSPECIFIED. ) 
 GEOMETRIC_REPRESENTATION_ITEM ( )  RATIONAL_B_SPLINE_SURFACE ( (
 ( 1.000000000000000000, 0.8047781103519398016, 1.000000000000000000),
 ( 1.000000000000000000, 0.8123785825774555436, 1.000000000000000000),
 ( 1.000000000000000000, 0.8190671539561653614, 1.000000000000000000),
 ( 1.000000000000000000, 0.8192352255061488009, 1.000000000000000000),
 ( 1.000000000000000000, 0.8126129677041400434, 1.000000000000000000),
 ( 1.000000000000000000, 0.8047712537969720081, 1.000000000000000000) ) ) 
 REPRESENTATION_ITEM ( '' )  SURFACE ( )  );
#389 = CARTESIAN_POINT ( 'NONE',  ( 1.560000000000005826, 0.8660254037844428154, 1.500000000000001332 ) ) ;
#390 = EDGE_CURVE ( 'NONE', #9890, #13868, #13175, .T. ) ;
#391 = DIRECTION ( 'NONE',  ( 0.000000000000000000, -0.000000000000000000, 1.000000000000000000 ) ) ;
#392 = CARTESIAN_POINT ( 'NONE',  ( 4.082498951862935321, 2.020725942163681399, 3.499999999999996003 ) ) ;
#393 = ORIENTED_EDGE ( 'NONE', *, *, #4064, .F. ) ;
#394 = CARTESIAN_POINT ( 'NONE',  ( -5.244818697407745312, 2.029379090245553741, -4.490884354499010023 ) ) ;
#395 = DIRECTION ( 'NONE',  ( 1.000000000000000000, 3.916739600140467622E-15, 0.000000000000000000 ) ) ;
#396 = AXIS2_PLACEMENT_3D ( 'NONE', #2897, #625, #12994 ) ;
#397 = DIRECTION ( 'NONE',  ( 0.000000000000000000, 0.000000000000000000, -1.000000000000000000 ) ) ;
#398 = ORIENTED_EDGE ( 'NONE', *, *, #479, .T. ) ;
#399 = CARTESIAN_POINT ( 'NONE',  ( 4.686019787951677174, -2.168404344971008868E-16, -4.000000000000015987 ) ) ;
#400 = ORIENTED_EDGE ( 'NONE', *, *, #1107, .F. ) ;
#401 = CARTESIAN_POINT ( 'NONE',  ( 6.800000000000028244, 1.327413925124860797E-15, 3.000000000000000000 ) ) ;
#402 = CARTESIAN_POINT ( 'NONE',  ( 20.00000000000000000, 47.00000000000000000, -25.00000000000000000 ) ) ;
#403 = ORIENTED_EDGE ( 'NONE', *, *, #3357, .F. ) ;
#404 = FACE_OUTER_BOUND ( 'NONE', #14317, .T. ) ;
#405 = DIRECTION ( 'NONE',  ( -1.000000000000000000, 0.000000000000000000, 0.000000000000000000 ) ) ;
#406 = EDGE_LOOP ( 'NONE', ( #12305, #13878, #13303, #2200 ) ) ;
#407 = DIRECTION ( 'NONE',  ( 0.000000000000000000, 0.000000000000000000, -1.000000000000000000 ) ) ;
#408 = VERTEX_POINT ( 'NONE', #8758 ) ;
#409 = EDGE_CURVE ( 'NONE', #3034, #3463, #1002, .T. ) ;
#410 = VECTOR ( 'NONE', #14385, 1000.000000000000000 ) ;
#411 = EDGE_LOOP ( 'NONE', ( #1168, #3751, #5257, #2145 ) ) ;
#412 = CARTESIAN_POINT ( 'NONE',  ( -140.0000000000003411, 189.5765550933606107, 47.99999999999998579 ) ) ;
#413 = DIRECTION ( 'NONE',  ( 0.000000000000000000, 0.000000000000000000, 1.000000000000000000 ) ) ;
#414 = CARTESIAN_POINT ( 'NONE',  ( -18.12748877629581656, 43.82334295289051340, 8.000000000000007105 ) ) ;
#415 = PRODUCT_DEFINITION_SHAPE ( 'NONE', 'NONE',  #11244 ) ;
#416 = CARTESIAN_POINT ( 'NONE',  ( 0.03421028094652689422, -3.072372537026350159, 2.678494666091049581 ) ) ;
#417 = SURFACE_STYLE_FILL_AREA ( #8158 ) ;
#418 = EDGE_CURVE ( 'NONE', #12547, #7049, #5258, .T. ) ;
#419 = CARTESIAN_POINT ( 'NONE',  ( 4.175813232069169878, 2.061359961916364725, -3.570380186727395433 ) ) ;
#420 = ITEM_DEFINED_TRANSFORMATION ( 'NONE', 'NONE', #3146,  #11025 ) ;
#421 = DIRECTION ( 'NONE',  ( 0.000000000000000000, 1.000000000000000000, 1.224646799147353207E-16 ) ) ;
#422 = B_SPLINE_CURVE_WITH_KNOTS ( 'NONE', 3,
 ( #9433, #5309, #10938, #9845, #3882, #8317, #12794, #9770 ),
 .UNSPECIFIED., .F., .F.,
 ( 4, 2, 2, 4 ),
 ( 0.005725059856848621793, 0.006314084072593604928, 0.006903108288338587195, 0.008081156719828553464 ),
 .UNSPECIFIED. ) ;
#423 = VECTOR ( 'NONE', #878, 1000.000000000000000 ) ;
#424 = CARTESIAN_POINT ( 'NONE',  ( -4.197312189423704432, -0.8182410726374524934, -3.202520316362464481 ) ) ;
#425 = DIRECTION ( 'NONE',  ( 0.000000000000000000, -1.000000000000000000, 0.000000000000000000 ) ) ;
#426 = VECTOR ( 'NONE', #4169, 1000.000000000000114 ) ;
#427 = DIRECTION ( 'NONE',  ( 1.000000000000000000, -2.312964634635743450E-16, -0.000000000000000000 ) ) ;
#428 = ORIENTED_EDGE ( 'NONE', *, *, #9517, .T. ) ;
#429 = EDGE_CURVE ( 'NONE', #1264, #5665, #1074, .T. ) ;
#430 = PRODUCT_RELATED_PRODUCT_CATEGORY ( 'part', '', ( #2643 ) ) ;
#431 = ORIENTED_EDGE ( 'NONE', *, *, #13902, .F. ) ;
#432 = LINE ( 'NONE', #11691, #9898 ) ;
#433 = VERTEX_POINT ( 'NONE', #855 ) ;
#434 = VECTOR ( 'NONE', #1179, 1000.000000000000000 ) ;
#435 = VERTEX_POINT ( 'NONE', #12201 ) ;
#436 = VECTOR ( 'NONE', #12555, 999.9999999999998863 ) ;
#437 = DIRECTION ( 'NONE',  ( 1.734723475976770502E-18, -4.440892098500621231E-16, -1.000000000000000000 ) ) ;
#438 = LINE ( 'NONE', #13839, #5839 ) ;
#439 = CARTESIAN_POINT ( 'NONE',  ( -108.6817075744280885, 39.57655509336044730, -117.0000000000000000 ) ) ;
#440 = AXIS2_PLACEMENT_3D ( 'NONE', #7787, #251, #5655 ) ;
#441 = CARTESIAN_POINT ( 'NONE',  ( -108.6817075744282590, 189.5765550933606107, 33.00000000000002842 ) ) ;
#442 = CARTESIAN_POINT ( 'NONE',  ( 139.9999999999996874, 199.5765550933606107, -132.0000000000000000 ) ) ;
#443 = CARTESIAN_POINT ( 'NONE',  ( 0.3126073911696169993, -2.020725942163681399, 3.499999999999989342 ) ) ;
#444 = DIRECTION ( 'NONE',  ( 0.000000000000000000, 0.000000000000000000, -1.000000000000000000 ) ) ;
#445 = CARTESIAN_POINT ( 'NONE',  ( 28.00000000000000355, 24.50000000000001421, 8.000000000000007105 ) ) ;
#446 = LINE ( 'NONE', #6057, #278 ) ;
#447 = COLOUR_RGB ( '', 0.72549020, 0.75294118, 0.79215686) ;
#448 = LINE ( 'NONE', #1383, #301 ) ;
#449 = ORIENTED_EDGE ( 'NONE', *, *, #10963, .T. ) ;
#450 = ORIENTED_EDGE ( 'NONE', *, *, #2914, .T. ) ;
#451 = B_SPLINE_CURVE_WITH_KNOTS ( 'NONE', 3,
 ( #1333, #11360, #8130, #1631, #322, #10560 ),
 .UNSPECIFIED., .F., .F.,
 ( 4, 2, 4 ),
 ( 0.000000000000000000, 0.002383230369971170957, 0.004766460739942341915 ),
 .UNSPECIFIED. ) ;
#452 = CARTESIAN_POINT ( 'NONE',  ( 4.071447262713911996, -4.041451884327377009, 0.000000000000000000 ) ) ;
#453 = DIRECTION ( 'NONE',  ( 0.000000000000000000, 0.000000000000000000, -1.000000000000000000 ) ) ;
#454 = VECTOR ( 'NONE', #10609, 1000.000000000000000 ) ;
#455 =( NAMED_UNIT ( * ) PLANE_ANGLE_UNIT ( ) SI_UNIT ( $, .RADIAN. ) );
#456 = ORIENTED_EDGE ( 'NONE', *, *, #10902, .F. ) ;
#457 = VECTOR ( 'NONE', #1303, 1000.000000000000000 ) ;
#458 =( REPRESENTATION_RELATIONSHIP ('NONE','NONE', #10295, #4961 ) REPRESENTATION_RELATIONSHIP_WITH_TRANSFORMATION ( #6919 )SHAPE_REPRESENTATION_RELATIONSHIP( ) );
#459 = ORIENTED_EDGE ( 'NONE', *, *, #3197, .T. ) ;
#460 = CARTESIAN_POINT ( 'NONE',  ( 3.514986608502051801, -4.017641317387857569, -4.357689166958506277 ) ) ;
#461 = CARTESIAN_POINT ( 'NONE',  ( 63.34848382498275754, 15.83712095624566984, 0.000000000000000000 ) ) ;
#462 = ORIENTED_EDGE ( 'NONE', *, *, #8769, .F. ) ;
#463 = DIRECTION ( 'NONE',  ( 1.000000000000000000, 1.723842398015259277E-15, -0.000000000000000000 ) ) ;
#464 = AXIS2_PLACEMENT_3D ( 'NONE', #1456, #12793, #10384 ) ;
#465 = EDGE_CURVE ( 'NONE', #9446, #7193, #8244, .T. ) ;
#466 = PRESENTATION_LAYER_ASSIGNMENT (  '', '', ( #1384 ) ) ;
#467 = CARTESIAN_POINT ( 'NONE',  ( -2.805705207896070252, 3.226868319750162861, -3.203898532754350104 ) ) ;
#468 = CARTESIAN_POINT ( 'NONE',  ( -129.3408537872145132, 189.5765550933606107, -75.00000000000001421 ) ) ;
#469 = CARTESIAN_POINT ( 'NONE',  ( 78.52142056027061301, -86.08568224108226730, -32.99999999999999289 ) ) ;
#470 = CARTESIAN_POINT ( 'NONE',  ( -25.00000000000000000, 199.5765550933606107, 47.99999999999998579 ) ) ;
#471 =( LENGTH_UNIT ( ) NAMED_UNIT ( * ) SI_UNIT ( .MILLI., .METRE. ) );
#472 = CARTESIAN_POINT ( 'NONE',  ( 0.7030283904629636149, 5.367609061414830407, -4.396693167833897853 ) ) ;
#473 = CARTESIAN_POINT ( 'NONE',  ( 4.851472949720994521, 1.539600717839003430, -4.000000000000002665 ) ) ;
#474 = ORIENTED_EDGE ( 'NONE', *, *, #4676, .T. ) ;
#475 = SURFACE_STYLE_FILL_AREA ( #10569 ) ;
#476 = VECTOR ( 'NONE', #6168, 1000.000000000000000 ) ;
#477 = ORIENTED_EDGE ( 'NONE', *, *, #13369, .F. ) ;
#478 = CARTESIAN_POINT ( 'NONE',  ( 5.384454397937120440, 8.966917871450958727E-16, -4.184454397937131809 ) ) ;
#479 = EDGE_CURVE ( 'NONE', #8503, #4363, #3283, .T. ) ;
#480 = CARTESIAN_POINT ( 'NONE',  ( -118.6817075744281595, 69.57655509336025546, -3.299999999999976730 ) ) ;
#481 = EDGE_LOOP ( 'NONE', ( #7301, #528 ) ) ;
#482 = PLANE ( 'NONE',  #7880 ) ;
#483 = DIRECTION ( 'NONE',  ( 0.000000000000000000, 0.000000000000000000, -1.000000000000000000 ) ) ;
#484 = ADVANCED_FACE ( 'NONE', ( #13027 ), #3077, .F. ) ;
#485 = CARTESIAN_POINT ( 'NONE',  ( 19.99999999999999645, 57.00000000000000000, 25.00000000000000000 ) ) ;
#486 = EDGE_LOOP ( 'NONE', ( #3660, #11536, #1623, #8148, #13235 ) ) ;
#487 =( GEOMETRIC_REPRESENTATION_CONTEXT ( 3 ) GLOBAL_UNCERTAINTY_ASSIGNED_CONTEXT ( ( #2963 ) ) GLOBAL_UNIT_ASSIGNED_CONTEXT ( ( #1746, #1885, #3068 ) ) REPRESENTATION_CONTEXT ( 'NONE', 'WORKASPACE' ) );
#488 = ORIENTED_EDGE ( 'NONE', *, *, #13152, .F. ) ;
#489 = VECTOR ( 'NONE', #4311, 1000.000000000000000 ) ;
#490 = DIRECTION ( 'NONE',  ( 1.000000000000000000, 0.000000000000000000, 0.000000000000000000 ) ) ;
#491 = DIRECTION ( 'NONE',  ( -2.081668171172169499E-16, 0.000000000000000000, 1.000000000000000000 ) ) ;
#492 = ORIENTED_EDGE ( 'NONE', *, *, #7099, .T. ) ;
#493 = CARTESIAN_POINT ( 'NONE',  ( 2.000000000000015543, 3.464101615137753942, 0.000000000000000000 ) ) ;
#494 = CARTESIAN_POINT ( 'NONE',  ( 49.55443476855437268, 62.09002498982675888, 25.00000000000000000 ) ) ;
#495 = DIRECTION ( 'NONE',  ( 1.000000000000000000, 0.000000000000000000, 0.000000000000000000 ) ) ;
#496 = SURFACE_STYLE_USAGE ( .BOTH. , #6408 ) ;
#497 = CARTESIAN_POINT ( 'NONE',  ( 129.3408537872138595, 199.5765550933606107, -13.99999999999999645 ) ) ;
#498 = CARTESIAN_POINT ( 'NONE',  ( 56.99999999999997868, -9.797174393178845379E-16, -25.00000000000000000 ) ) ;
#499 = EDGE_CURVE ( 'NONE', #10194, #2629, #8920, .T. ) ;
#500 = VECTOR ( 'NONE', #1584, 1000.000000000000000 ) ;
#501 = DIRECTION ( 'NONE',  ( 0.000000000000000000, 0.000000000000000000, -1.000000000000000000 ) ) ;
#502 = DIRECTION ( 'NONE',  ( -0.000000000000000000, -0.000000000000000000, -1.000000000000000000 ) ) ;
#503 = AXIS2_PLACEMENT_3D ( 'NONE', #5425, #10035, #883 ) ;
#504 = EDGE_LOOP ( 'NONE', ( #9711, #6187, #8657, #5376, #2686 ) ) ;
#505 = CARTESIAN_POINT ( 'NONE',  ( -108.6817075744280174, -30.42344490663958112, 47.99999999999998579 ) ) ;
#506 = ORIENTED_EDGE ( 'NONE', *, *, #6821, .T. ) ;
#507 = CIRCLE ( 'NONE', #2371, 2.750000000000003997 ) ;
#508 = ORIENTED_EDGE ( 'NONE', *, *, #6035, .F. ) ;
#509 = LINE ( 'NONE', #9432, #9588 ) ;
#510 = PRESENTATION_LAYER_ASSIGNMENT (  '', '', ( #2372 ) ) ;
#511 = AXIS2_PLACEMENT_3D ( 'NONE', #2346, #91, #4566 ) ;
#512 = LINE ( 'NONE', #14249, #3944 ) ;
#513 = LINE ( 'NONE', #8482, #11201 ) ;
#514 = LINE ( 'NONE', #5974, #2322 ) ;
#515 = CARTESIAN_POINT ( 'NONE',  ( 5.046772446839304926, -2.317775331972803610, -4.014504635506726871 ) ) ;
#516 = ORIENTED_EDGE ( 'NONE', *, *, #14434, .F. ) ;
#517 = CARTESIAN_POINT ( 'NONE',  ( 4.071447262713911996, -2.020725942163681399, -3.500000000000010214 ) ) ;
#518 = DIRECTION ( 'NONE',  ( -1.000000000000000000, 0.000000000000000000, 0.000000000000000000 ) ) ;
#519 = CARTESIAN_POINT ( 'NONE',  ( 2.500000000000018652, 4.330127018922186544, 0.000000000000000000 ) ) ;
#520 = ADVANCED_FACE ( 'NONE', ( #9180 ), #8896, .T. ) ;
#521 = CARTESIAN_POINT ( 'NONE',  ( 28.00000000000000355, 29.99999999999999645, -5.738192700042120897 ) ) ;
#522 = EDGE_CURVE ( 'NONE', #47, #5931, #7516, .T. ) ;
#523 = VECTOR ( 'NONE', #2168, 1000.000000000000000 ) ;
#524 = VECTOR ( 'NONE', #14360, 1000.000000000000000 ) ;
#525 = CIRCLE ( 'NONE', #4047, 2.749999999999997780 ) ;
#526 = DIRECTION ( 'NONE',  ( 1.000000000000000000, 1.665334536937734318E-16, 0.000000000000000000 ) ) ;
#527 = ORIENTED_EDGE ( 'NONE', *, *, #10032, .F. ) ;
#528 = ORIENTED_EDGE ( 'NONE', *, *, #1670, .T. ) ;
#529 = EDGE_LOOP ( 'NONE', ( #11917, #4776, #6144, #12759 ) ) ;
#530 = FACE_BOUND ( 'NONE', #4280, .T. ) ;
#531 = FACE_OUTER_BOUND ( 'NONE', #7015, .T. ) ;
#532 =( GEOMETRIC_REPRESENTATION_CONTEXT ( 3 ) GLOBAL_UNCERTAINTY_ASSIGNED_CONTEXT ( ( #5003 ) ) GLOBAL_UNIT_ASSIGNED_CONTEXT ( ( #13584, #179, #1134 ) ) REPRESENTATION_CONTEXT ( 'NONE', 'WORKASPACE' ) );
#533 = VECTOR ( 'NONE', #11200, 1000.000000000000000 ) ;
#534 =( NAMED_UNIT ( * ) SI_UNIT ( $, .STERADIAN. ) SOLID_ANGLE_UNIT ( ) );
#535 = VERTEX_POINT ( 'NONE', #5729 ) ;
#536 = CARTESIAN_POINT ( 'NONE',  ( 37.35300976710104948, 100.8957249956400375, -25.00000000000000000 ) ) ;
#537 = FACE_OUTER_BOUND ( 'NONE', #8582, .T. ) ;
#538 = ORIENTED_EDGE ( 'NONE', *, *, #8944, .T. ) ;
#539 = DIRECTION ( 'NONE',  ( 0.000000000000000000, 0.000000000000000000, -1.000000000000000000 ) ) ;
#540 = AXIS2_PLACEMENT_3D ( 'NONE', #6567, #938, #12142 ) ;
#541 = ORIENTED_EDGE ( 'NONE', *, *, #11559, .T. ) ;
#542 = LINE ( 'NONE', #11735, #3309 ) ;
#543 = CARTESIAN_POINT ( 'NONE',  ( 30.10000000000000497, 29.99999999999999645, 6.999999999999992006 ) ) ;
#544 = LINE ( 'NONE', #5067, #7395 ) ;
#545 = ORIENTED_EDGE ( 'NONE', *, *, #4939, .T. ) ;
#546 = CARTESIAN_POINT ( 'NONE',  ( 0.8333333333333354798, 5.292377467571581562, -4.118275046351174140 ) ) ;
#547 = CARTESIAN_POINT ( 'NONE',  ( 22.00000000000000355, 27.00000000000000355, -25.00000000000000000 ) ) ;
#548 = PRESENTATION_STYLE_ASSIGNMENT (( #10489 ) ) ;
#549 = VERTEX_POINT ( 'NONE', #5876 ) ;
#550 = CARTESIAN_POINT ( 'NONE',  ( 4.319324222800557500, 3.279739689145082959, -4.138711833383065475 ) ) ;
#551 = ORIENTED_EDGE ( 'NONE', *, *, #3076, .F. ) ;
#552 = APPLICATION_CONTEXT ( 'automotive_design' ) ;
#553 = FACE_OUTER_BOUND ( 'NONE', #9521, .T. ) ;
#554 = AXIS2_PLACEMENT_3D ( 'NONE', #7102, #318, #1552 ) ;
#555 = ORIENTED_EDGE ( 'NONE', *, *, #8079, .T. ) ;
#556 = EDGE_CURVE ( 'NONE', #7883, #4518, #5673, .T. ) ;
#557 = ADVANCED_FACE ( 'NONE', ( #2536 ), #12548, .F. ) ;
#558 = ORIENTED_EDGE ( 'NONE', *, *, #7367, .T. ) ;
#559 = CARTESIAN_POINT ( 'NONE',  ( 1.432312439535594395, 4.946556719366753896, -0.1121614189353446478 ) ) ;
#560 = LINE ( 'NONE', #11665, #13855 ) ;
#561 = AXIS2_PLACEMENT_3D ( 'NONE', #10302, #7885, #290 ) ;
#562 = VERTEX_POINT ( 'NONE', #3500 ) ;
#563 = CARTESIAN_POINT ( 'NONE',  ( 61.60657227073433262, 3.881474981106830313, 25.00000000000000000 ) ) ;
#564 = FACE_BOUND ( 'NONE', #13096, .T. ) ;
#565 = AXIS2_PLACEMENT_3D ( 'NONE', #9439, #3818, #518 ) ;
#566 = DIRECTION ( 'NONE',  ( 0.000000000000000000, 0.000000000000000000, 1.000000000000000000 ) ) ;
#567 = ORIENTED_EDGE ( 'NONE', *, *, #1776, .F. ) ;
#568 = VERTEX_POINT ( 'NONE', #13389 ) ;
#569 = CARTESIAN_POINT ( 'NONE',  ( 2.949999999999994404, 0.000000000000000000, 0.000000000000000000 ) ) ;
#570 = CARTESIAN_POINT ( 'NONE',  ( -25.00000000000000000, -30.42444490663959300, 47.99999999999998579 ) ) ;
#571 = EDGE_CURVE ( 'NONE', #8706, #2255, #3695, .T. ) ;
#572 = ORIENTED_EDGE ( 'NONE', *, *, #5224, .F. ) ;
#573 = LINE ( 'NONE', #10585, #7006 ) ;
#574 = CARTESIAN_POINT ( 'NONE',  ( -108.6817075744280174, -30.42344490663958112, 33.00000000000002842 ) ) ;
#575 = CARTESIAN_POINT ( 'NONE',  ( 79.68170757442804586, 124.5765550933606249, 25.00000000000000000 ) ) ;
#576 = PLANE ( 'NONE',  #3995 ) ;
#577 = ADVANCED_FACE ( 'NONE', ( #191 ), #8077, .F. ) ;
#578 = ORIENTED_EDGE ( 'NONE', *, *, #4864, .T. ) ;
#579 = CARTESIAN_POINT ( 'NONE',  ( 1.560000000000005826, -1.732050807568885631, 0.000000000000000000 ) ) ;
#580 = EDGE_CURVE ( 'NONE', #10243, #2320, #2923, .T. ) ;
#581 = CARTESIAN_POINT ( 'NONE',  ( 0.000000000000000000, 0.000000000000000000, 35.00000000000000000 ) ) ;
#582 = PLANE ( 'NONE',  #287 ) ;
#583 = CARTESIAN_POINT ( 'NONE',  ( -0.8082922630888625948, -5.306834936218045584, -0.2701150775514032376 ) ) ;
#584 = ADVANCED_FACE ( 'NONE', ( #10851 ), #6393, .T. ) ;
#585 = ORIENTED_EDGE ( 'NONE', *, *, #12122, .F. ) ;
#586 = ORIENTED_EDGE ( 'NONE', *, *, #1107, .T. ) ;
#587 = DIRECTION ( 'NONE',  ( -0.2425356250363328581, 0.9701425001453318764, -0.000000000000000000 ) ) ;
#588 = VERTEX_POINT ( 'NONE', #1353 ) ;
#589 = EDGE_CURVE ( 'NONE', #11502, #1350, #7940, .T. ) ;
#590 = EDGE_LOOP ( 'NONE', ( #10183, #10627, #12842, #12199 ) ) ;
#591 = CARTESIAN_POINT ( 'NONE',  ( 30.00229726637438432, 120.2985749985466839, -25.00000000000000000 ) ) ;
#592 = B_SPLINE_CURVE_WITH_KNOTS ( 'NONE', 3,
 ( #1588, #2278, #11199, #5965, #2620, #12712 ),
 .UNSPECIFIED., .F., .F.,
 ( 4, 2, 4 ),
 ( -3.640115492423102241E-06, 0.0002066546034006423217, 0.0004169493222937077355 ),
 .UNSPECIFIED. ) ;
#593 = CARTESIAN_POINT ( 'NONE',  ( 6.799999999999972289, -2.309401076758498039, -4.000000000000003553 ) ) ;
#594 = LINE ( 'NONE', #11851, #8147 ) ;
#595 = CARTESIAN_POINT ( 'NONE',  ( 79.68170757442804586, 59.57655509336061073, -25.00000000000000000 ) ) ;
#596 = DIRECTION ( 'NONE',  ( -1.000000000000000000, 0.000000000000000000, 0.000000000000000000 ) ) ;
#597 = ORIENTED_EDGE ( 'NONE', *, *, #130, .F. ) ;
#598 = CARTESIAN_POINT ( 'NONE',  ( 1.560000000000005826, 0.000000000000000000, 0.000000000000000000 ) ) ;
#599 = CARTESIAN_POINT ( 'NONE',  ( 99.68170757442806007, 69.57655509336045441, 1.591964985538234261E-14 ) ) ;
#600 = FACE_BOUND ( 'NONE', #2682, .T. ) ;
#601 = EDGE_CURVE ( 'NONE', #11659, #3422, #11541, .T. ) ;
#602 = CARTESIAN_POINT ( 'NONE',  ( 108.6817075744280459, 189.5765550933606107, -106.9999999999999858 ) ) ;
#603 = DIRECTION ( 'NONE',  ( 0.000000000000000000, -5.551115123125782702E-17, -1.000000000000000000 ) ) ;
#604 = ORIENTED_EDGE ( 'NONE', *, *, #5491, .T. ) ;
#605 = ORIENTED_EDGE ( 'NONE', *, *, #10788, .F. ) ;
#606 = VECTOR ( 'NONE', #3848, 1000.000000000000000 ) ;
#607 = EDGE_CURVE ( 'NONE', #7346, #10278, #2254, .T. ) ;
#608 = ORIENTED_EDGE ( 'NONE', *, *, #7283, .F. ) ;
#609 = DIRECTION ( 'NONE',  ( 0.000000000000000000, -1.000000000000000000, 0.000000000000000000 ) ) ;
#610 = CARTESIAN_POINT ( 'NONE',  ( 28.00000000000000355, 29.99999999999999645, 8.000000000000007105 ) ) ;
#611 = SURFACE_STYLE_USAGE ( .BOTH. , #8196 ) ;
#612 = ORIENTED_EDGE ( 'NONE', *, *, #11829, .T. ) ;
#613 = ORIENTED_EDGE ( 'NONE', *, *, #4304, .T. ) ;
#614 = CARTESIAN_POINT ( 'NONE',  ( 54.25585977000769589, 23.28432498401347672, 25.00000000000000000 ) ) ;
#615 = AXIS2_PLACEMENT_3D ( 'NONE', #11565, #1541, #13643 ) ;
#616 = DIRECTION ( 'NONE',  ( -0.3822382184081045131, -0.9240638205168505426, 0.000000000000000000 ) ) ;
#617 = ORIENTED_EDGE ( 'NONE', *, *, #13492, .F. ) ;
#618 = FACE_OUTER_BOUND ( 'NONE', #7794, .T. ) ;
#619 = VERTEX_POINT ( 'NONE', #10072 ) ;
#620 = EDGE_CURVE ( 'NONE', #11306, #10601, #10148, .T. ) ;
#621 = UNCERTAINTY_MEASURE_WITH_UNIT (LENGTH_MEASURE( 1.000000000000000082E-05 ), #3972, 'distance_accuracy_value', 'NONE');
#622 = ADVANCED_FACE ( 'NONE', ( #129 ), #8970, .F. ) ;
#623 = FACE_OUTER_BOUND ( 'NONE', #7220, .T. ) ;
#624 = CARTESIAN_POINT ( 'NONE',  ( 0.02993401039713497816, -3.373851915354613151, -1.156317065392235222 ) ) ;
#625 = DIRECTION ( 'NONE',  ( 0.000000000000000000, 0.000000000000000000, 1.000000000000000000 ) ) ;
#626 = EDGE_LOOP ( 'NONE', ( #10160, #3816, #10628, #10696 ) ) ;
#627 = CARTESIAN_POINT ( 'NONE',  ( 5.733169058567799681, -3.291357029458752715E-15, 6.438111078829122036 ) ) ;
#628 = LINE ( 'NONE', #5290, #3064 ) ;
#629 =( NAMED_UNIT ( * ) SI_UNIT ( $, .STERADIAN. ) SOLID_ANGLE_UNIT ( ) );
#630 = VERTEX_POINT ( 'NONE', #2390 ) ;
#631 = CARTESIAN_POINT ( 'NONE',  ( -108.6817075744279748, 39.57655509336049704, -106.9999999999999858 ) ) ;
#632 = B_SPLINE_CURVE_WITH_KNOTS ( 'NONE', 3,
 ( #2328, #11388, #8022, #3652, #12358, #8979 ),
 .UNSPECIFIED., .F., .F.,
 ( 4, 2, 4 ),
 ( 0.002950759650825622842, 0.004429055062152257617, 0.005907350473478891958 ),
 .UNSPECIFIED. ) ;
#633 = DIRECTION ( 'NONE',  ( 1.000000000000000000, 2.312964634635743943E-16, 0.000000000000000000 ) ) ;
#634 = ORIENTED_EDGE ( 'NONE', *, *, #1889, .T. ) ;
#635 = DIRECTION ( 'NONE',  ( 0.000000000000000000, 0.000000000000000000, 1.000000000000000000 ) ) ;
#636 = CARTESIAN_POINT ( 'NONE',  ( -108.6817075744279748, 29.57655509336048993, -106.9999999999999858 ) ) ;
#637 = ORIENTED_EDGE ( 'NONE', *, *, #8722, .T. ) ;
#638 = CARTESIAN_POINT ( 'NONE',  ( 31.24550000000003536, -9.697272942312978198E-16, -3.000000000000000000 ) ) ;
#639 = CARTESIAN_POINT ( 'NONE',  ( -4.000000000000000000, -2.309401076758511806, -3.133295621305376422 ) ) ;
#640 = CARTESIAN_POINT ( 'NONE',  ( 5.056385618527004411, 4.642911450026675269, 0.000000000000000000 ) ) ;
#641 = VERTEX_POINT ( 'NONE', #6850 ) ;
#642 = EDGE_LOOP ( 'NONE', ( #3590, #6083 ) ) ;
#643 = PLANE ( 'NONE',  #7331 ) ;
#644 = CARTESIAN_POINT ( 'NONE',  ( -108.6817075744282448, 109.5765550933602839, -3.299999999999976730 ) ) ;
#645 = APPLICATION_CONTEXT ( 'automotive_design' ) ;
#646 = ORIENTED_EDGE ( 'NONE', *, *, #11385, .F. ) ;
#647 = LINE ( 'NONE', #4099, #15 ) ;
#648 = DIRECTION ( 'NONE',  ( 0.000000000000000000, 0.000000000000000000, -1.000000000000000000 ) ) ;
#649 = ORIENTED_EDGE ( 'NONE', *, *, #239, .T. ) ;
#650 = LINE ( 'NONE', #12861, #14230 ) ;
#651 = VERTEX_POINT ( 'NONE', #11316 ) ;
#652 = FILL_AREA_STYLE_COLOUR ( '', #8179 ) ;
#653 = CARTESIAN_POINT ( 'NONE',  ( 0.000000000000000000, 2.375000000000000000, 0.000000000000000000 ) ) ;
#654 = DIRECTION ( 'NONE',  ( 0.7071067811865467956, -0.7071067811865483499, -0.000000000000000000 ) ) ;
#655 = CARTESIAN_POINT ( 'NONE',  ( 5.733169058567799681, -3.291357029458752715E-15, 6.438111078829122036 ) ) ;
#656 = AXIS2_PLACEMENT_3D ( 'NONE', #5018, #7273, #14033 ) ;
#657 = ORIENTED_EDGE ( 'NONE', *, *, #4198, .F. ) ;
#658 = VERTEX_POINT ( 'NONE', #8455 ) ;
#659 = ADVANCED_FACE ( 'NONE', ( #12942 ), #643, .F. ) ;
#660 = LINE ( 'NONE', #2704, #1726 ) ;
#661 = VERTEX_POINT ( 'NONE', #10362 ) ;
#662 = EDGE_CURVE ( 'NONE', #4679, #9332, #11674, .T. ) ;
#663 = VERTEX_POINT ( 'NONE', #11528 ) ;
#664 = DIRECTION ( 'NONE',  ( -1.000000000000000000, -1.665334536937734071E-16, 0.000000000000000000 ) ) ;
#665 = PLANE ( 'NONE',  #4214 ) ;
#666 = AXIS2_PLACEMENT_3D ( 'NONE', #7553, #831, #14236 ) ;
#667 = CARTESIAN_POINT ( 'NONE',  ( 2.450325270861126281, 48.11882021490242778, 7.172319002129951215 ) ) ;
#668 = LINE ( 'NONE', #3960, #5178 ) ;
#669 = AXIS2_PLACEMENT_3D ( 'NONE', #11683, #2851, #792 ) ;
#670 = DIRECTION ( 'NONE',  ( -3.916739600140467622E-15, 1.000000000000000000, 0.000000000000000000 ) ) ;
#671 = APPLICATION_PROTOCOL_DEFINITION ( 'draft international standard', 'automotive_design', 1998, #7823 ) ;
#672 = CARTESIAN_POINT ( 'NONE',  ( 31.80000000000005045, 8.024914066595556114E-15, 2.445500000000030649 ) ) ;
#673 = CARTESIAN_POINT ( 'NONE',  ( 3.950241966888151879, -3.393956070637468958, 1.121495646998917017 ) ) ;
#674 = EDGE_CURVE ( 'NONE', #2739, #5618, #12700, .T. ) ;
#675 = CYLINDRICAL_SURFACE ( 'NONE', #9158, 4.999999999999976907 ) ;
#676 = VECTOR ( 'NONE', #9454, 1000.000000000000000 ) ;
#677 = VECTOR ( 'NONE', #3560, 999.9999999999998863 ) ;
#678 = VECTOR ( 'NONE', #13825, 1000.000000000000000 ) ;
#679 = EDGE_CURVE ( 'NONE', #13538, #9142, #13956, .T. ) ;
#680 = ORIENTED_EDGE ( 'NONE', *, *, #3167, .T. ) ;
#681 = CARTESIAN_POINT ( 'NONE',  ( 22.00000000000000000, 60.00000000000000711, 25.00000000000000000 ) ) ;
#682 = DIRECTION ( 'NONE',  ( 0.000000000000000000, 0.000000000000000000, 1.000000000000000000 ) ) ;
#683 = ORIENTED_EDGE ( 'NONE', *, *, #8121, .T. ) ;
#684 = CARTESIAN_POINT ( 'NONE',  ( 62.10586122665984732, -20.42344490663941414, 35.00000000000000000 ) ) ;
#685 = EDGE_CURVE ( 'NONE', #3184, #7164, #14140, .T. ) ;
#686 = CARTESIAN_POINT ( 'NONE',  ( -3.401922400370679167, -3.809401878279965015, -4.271474537230584900 ) ) ;
#687 = VERTEX_POINT ( 'NONE', #13818 ) ;
#688 = CARTESIAN_POINT ( 'NONE',  ( 92.68170757442806007, 124.5765550933605965, 25.00000000000000000 ) ) ;
#689 = CARTESIAN_POINT ( 'NONE',  ( 64.03192852109765454, -5.819950020346492892, 25.00000000000000000 ) ) ;
#690 = CARTESIAN_POINT ( 'NONE',  ( 0.000000000000000000, 40.49999999999999289, 8.000000000000007105 ) ) ;
#691 = CARTESIAN_POINT ( 'NONE',  ( 30.10000000000000497, 29.99999999999999645, -6.999999999999992006 ) ) ;
#692 = ORIENTED_EDGE ( 'NONE', *, *, #7072, .F. ) ;
#693 = CARTESIAN_POINT ( 'NONE',  ( -5.236872748402765509, -8.016972670139777574E-14, -4.357689166958463645 ) ) ;
#694 = FACE_BOUND ( 'NONE', #11112, .T. ) ;
#695 = PRESENTATION_LAYER_ASSIGNMENT (  '', '', ( #3974 ) ) ;
#696 = VERTEX_POINT ( 'NONE', #8297 ) ;
#697 = CARTESIAN_POINT ( 'NONE',  ( -1.734723475976807094E-14, 35.49999999999996447, 8.000000000000007105 ) ) ;
#698 = VERTEX_POINT ( 'NONE', #3713 ) ;
#699 = CARTESIAN_POINT ( 'NONE',  ( -28.00000000000000355, 24.50000000000001421, 0.000000000000000000 ) ) ;
#700 = CARTESIAN_POINT ( 'NONE',  ( 22.00000000000000355, 40.00000000000000711, -25.00000000000000000 ) ) ;
#701 = ADVANCED_FACE ( 'NONE', ( #4946 ), #3933, .T. ) ;
#702 = ADVANCED_FACE ( 'NONE', ( #11758 ), #12020, .F. ) ;
#703 = DIRECTION ( 'NONE',  ( 0.2425356250363328581, -0.9701425001453318764, -0.000000000000000000 ) ) ;
#704 = VECTOR ( 'NONE', #1188, 1000.000000000000000 ) ;
#705 = ORIENTED_EDGE ( 'NONE', *, *, #5491, .F. ) ;
#706 = DIRECTION ( 'NONE',  ( 0.000000000000000000, 0.000000000000000000, 1.000000000000000000 ) ) ;
#707 = FACE_BOUND ( 'NONE', #8200, .T. ) ;
#708 = ORIENTED_EDGE ( 'NONE', *, *, #1688, .T. ) ;
#709 = LINE ( 'NONE', #5166, #6863 ) ;
#710 = DIRECTION ( 'NONE',  ( 0.000000000000000000, 0.000000000000000000, -1.000000000000000000 ) ) ;
#711 = EDGE_LOOP ( 'NONE', ( #8770, #6169 ) ) ;
#712 = CARTESIAN_POINT ( 'NONE',  ( 3.878096787214415198, 2.680238624820971083, -2.357690525401547443 ) ) ;
#713 = AXIS2_PLACEMENT_3D ( 'NONE', #14232, #7612, #6386 ) ;
#714 = CARTESIAN_POINT ( 'NONE',  ( -88.22284556172397174, 29.57655509336047572, -106.9999999999999858 ) ) ;
#715 = CARTESIAN_POINT ( 'NONE',  ( 20.00000000000000000, -5.510910596163090344E-15, 25.00000000000000000 ) ) ;
#716 = VERTEX_POINT ( 'NONE', #7054 ) ;
#717 = DIRECTION ( 'NONE',  ( 0.000000000000000000, 0.000000000000000000, 1.000000000000000000 ) ) ;
#718 = DIRECTION ( 'NONE',  ( -1.000000000000000000, 0.000000000000000000, 0.000000000000000000 ) ) ;
#719 = DIRECTION ( 'NONE',  ( -0.000000000000000000, 1.000000000000000000, 0.000000000000000000 ) ) ;
#720 = VECTOR ( 'NONE', #4602, 1000.000000000000000 ) ;
#721 = VERTEX_POINT ( 'NONE', #10426 ) ;
#722 = DIRECTION ( 'NONE',  ( 0.000000000000000000, 0.000000000000000000, 1.000000000000000000 ) ) ;
#723 = ORIENTED_EDGE ( 'NONE', *, *, #10769, .F. ) ;
#724 = ORIENTED_EDGE ( 'NONE', *, *, #11650, .F. ) ;
#725 = DIRECTION ( 'NONE',  ( 0.000000000000000000, -1.000000000000000000, 0.000000000000000000 ) ) ;
#726 = DIRECTION ( 'NONE',  ( 0.000000000000000000, 4.440892098500620738E-16, 1.000000000000000000 ) ) ;
#727 = DIRECTION ( 'NONE',  ( -0.9701425001453319874, -0.2425356250363328026, 0.000000000000000000 ) ) ;
#728 = CONICAL_SURFACE ( 'NONE', #12412, 2.054999999999999716, 0.7853981633974428389 ) ;
#729 = DIRECTION ( 'NONE',  ( 0.000000000000000000, 0.000000000000000000, -1.000000000000000000 ) ) ;
#730 = VECTOR ( 'NONE', #6841, 1000.000000000000000 ) ;
#731 = LINE ( 'NONE', #8625, #5410 ) ;
#732 = APPLICATION_PROTOCOL_DEFINITION ( 'draft international standard', 'automotive_design', 1998, #12786 ) ;
#733 = DIRECTION ( 'NONE',  ( 0.2425356250363330801, -0.9701425001453319874, -0.000000000000000000 ) ) ;
#734 = AXIS2_PLACEMENT_3D ( 'NONE', #1571, #11524, #13887 ) ;
#735 = CARTESIAN_POINT ( 'NONE',  ( 3.903127820947815962E-15, 5.773502691896270633, -0.5999999999999894307 ) ) ;
#736 = ADVANCED_FACE ( 'NONE', ( #5952 ), #4871, .T. ) ;
#737 = ORIENTED_EDGE ( 'NONE', *, *, #6925, .T. ) ;
#738 = CARTESIAN_POINT ( 'NONE',  ( 0.000000000000000000, 0.000000000000000000, -4.394516984716101859 ) ) ;
#739 = AXIS2_PLACEMENT_3D ( 'NONE', #9438, #3738, #8183 ) ;
#740 = AXIS2_PLACEMENT_3D ( 'NONE', #6657, #8927, #12156 ) ;
#741 = ORIENTED_EDGE ( 'NONE', *, *, #8946, .F. ) ;
#742 = EDGE_CURVE ( 'NONE', #5183, #3543, #1654, .T. ) ;
#743 =( REPRESENTATION_RELATIONSHIP ('NONE','NONE', #10295, #10940 ) REPRESENTATION_RELATIONSHIP_WITH_TRANSFORMATION ( #13400 )SHAPE_REPRESENTATION_RELATIONSHIP( ) );
#744 = ORIENTED_EDGE ( 'NONE', *, *, #1270, .T. ) ;
#745 = CARTESIAN_POINT ( 'NONE',  ( 105.6817075744281311, 124.5765550933606107, 25.00000000000000000 ) ) ;
#746 = LINE ( 'NONE', #10695, #6564 ) ;
#747 = EDGE_CURVE ( 'NONE', #10823, #25, #10507, .T. ) ;
#748 = ORIENTED_EDGE ( 'NONE', *, *, #2973, .T. ) ;
#749 = VECTOR ( 'NONE', #1705, 1000.000000000000000 ) ;
#750 = AXIS2_PLACEMENT_3D ( 'NONE', #4185, #13245, #6639 ) ;
#751 = EDGE_CURVE ( 'NONE', #8097, #29, #10582, .T. ) ;
#752 = LINE ( 'NONE', #6297, #3942 ) ;
#753 = CARTESIAN_POINT ( 'NONE',  ( 56.99999999999997868, -9.797174393178845379E-16, -25.00000000000000000 ) ) ;
#754 = ORIENTED_EDGE ( 'NONE', *, *, #2268, .T. ) ;
#755 = DIRECTION ( 'NONE',  ( 0.9701425001453319874, 0.2425356250363328858, -0.000000000000000000 ) ) ;
#756 = EDGE_CURVE ( 'NONE', #6205, #7193, #7281, .T. ) ;
#757 = ORIENTED_EDGE ( 'NONE', *, *, #2376, .F. ) ;
#758 =( GEOMETRIC_REPRESENTATION_CONTEXT ( 3 ) GLOBAL_UNCERTAINTY_ASSIGNED_CONTEXT ( ( #7174 ) ) GLOBAL_UNIT_ASSIGNED_CONTEXT ( ( #1276, #6755, #8134 ) ) REPRESENTATION_CONTEXT ( 'NONE', 'WORKASPACE' ) );
#759 = UNCERTAINTY_MEASURE_WITH_UNIT (LENGTH_MEASURE( 1.000000000000000082E-05 ), #7893, 'distance_accuracy_value', 'NONE');
#760 = CIRCLE ( 'NONE', #8929, 2.000000000000001776 ) ;
#761 = LINE ( 'NONE', #12029, #4486 ) ;
#762 = DIRECTION ( 'NONE',  ( 0.8571673007021134438, 1.049727191138620051E-16, -0.5150380749100522682 ) ) ;
#763 = CARTESIAN_POINT ( 'NONE',  ( 0.000000000000000000, 2.081668171172168513E-14, 4.000000000000003553 ) ) ;
#764 = EDGE_LOOP ( 'NONE', ( #5468, #4866, #1029, #12657, #7119, #9076, #4306, #10621 ) ) ;
#765 = ADVANCED_FACE ( 'NONE', ( #2762 ), #11597, .T. ) ;
#766 = CARTESIAN_POINT ( 'NONE',  ( 30.60000000000001563, 1.140754157802348188E-16, 2.054999999999999716 ) ) ;
#767 = LINE ( 'NONE', #826, #476 ) ;
#768 = VERTEX_POINT ( 'NONE', #5023 ) ;
#769 = DIRECTION ( 'NONE',  ( 0.000000000000000000, 1.000000000000000000, 0.000000000000000000 ) ) ;
#770 = ORIENTED_EDGE ( 'NONE', *, *, #14399, .F. ) ;
#771 = ORIENTED_EDGE ( 'NONE', *, *, #1381, .F. ) ;
#772 = CARTESIAN_POINT ( 'NONE',  ( 2.500000000000018652, 4.330127018922186544, 0.000000000000000000 ) ) ;
#773 = EDGE_CURVE ( 'NONE', #12337, #11431, #4564, .T. ) ;
#774 = VECTOR ( 'NONE', #10253, 1000.000000000000000 ) ;
#775 = VECTOR ( 'NONE', #609, 1000.000000000000000 ) ;
#776 = CARTESIAN_POINT ( 'NONE',  ( 5.599999999999994316, 4.041451884327390331, 0.000000000000000000 ) ) ;
#777 = VERTEX_POINT ( 'NONE', #1804 ) ;
#778 = CARTESIAN_POINT ( 'NONE',  ( 71.80728622811317052, -17.99808865627607801, 28.00000000000000000 ) ) ;
#779 = LINE ( 'NONE', #3128, #5895 ) ;
#780 = VERTEX_POINT ( 'NONE', #341 ) ;
#781 = ORIENTED_EDGE ( 'NONE', *, *, #5427, .F. ) ;
#782 = CARTESIAN_POINT ( 'NONE',  ( 3.806834918298607651, 8.673617379884035472E-16, -3.499999999999975131 ) ) ;
#783 = CARTESIAN_POINT ( 'NONE',  ( -0.4317663827706254565, -5.811727376006682988, -4.566919140436432656 ) ) ;
#784 = EDGE_CURVE ( 'NONE', #562, #2174, #4802, .T. ) ;
#785 = ORIENTED_EDGE ( 'NONE', *, *, #8014, .F. ) ;
#786 = CARTESIAN_POINT ( 'NONE',  ( 4.124214193018064911, -4.056676826581889550, -6.938408812827713022E-15 ) ) ;
#787 = AXIS2_PLACEMENT_3D ( 'NONE', #5564, #10033, #8932 ) ;
#788 = PLANE ( 'NONE',  #1131 ) ;
#789 = FACE_OUTER_BOUND ( 'NONE', #1160, .T. ) ;
#790 = CARTESIAN_POINT ( 'NONE',  ( 3.972058292797703949, 0.6948821373597541262, 3.565770528409232920 ) ) ;
#791 = ORIENTED_EDGE ( 'NONE', *, *, #5224, .T. ) ;
#792 = DIRECTION ( 'NONE',  ( -1.000000000000000000, 0.000000000000000000, 0.000000000000000000 ) ) ;
#793 = CYLINDRICAL_SURFACE ( 'NONE', #14229, 2.500000000000002220 ) ;
#794 = ORIENTED_EDGE ( 'NONE', *, *, #7642, .F. ) ;
#795 = DIRECTION ( 'NONE',  ( 1.000000000000000000, 0.000000000000000000, 0.000000000000000000 ) ) ;
#796 = EDGE_CURVE ( 'NONE', #3727, #13520, #8809, .T. ) ;
#797 = EDGE_LOOP ( 'NONE', ( #4889, #11976, #11139, #14129 ) ) ;
#798 = CARTESIAN_POINT ( 'NONE',  ( 76.68170757442801744, 39.57655509336063204, -33.00000000000000000 ) ) ;
#799 = EDGE_CURVE ( 'NONE', #14126, #11064, #3187, .T. ) ;
#800 = DIRECTION ( 'NONE',  ( -1.000000000000000000, 0.000000000000000000, 0.000000000000000000 ) ) ;
#801 = AXIS2_PLACEMENT_3D ( 'NONE', #2418, #4974, #7008 ) ;
#802 = CARTESIAN_POINT ( 'NONE',  ( 4.000000000000003553, 2.309401076758501592, -3.133295621305376422 ) ) ;
#803 = DIRECTION ( 'NONE',  ( 0.000000000000000000, -8.482162385747133845E-47, 1.000000000000000000 ) ) ;
#804 = APPLICATION_PROTOCOL_DEFINITION ( 'draft international standard', 'automotive_design', 1998, #3629 ) ;
#805 = CARTESIAN_POINT ( 'NONE',  ( 0.3572655899081733644, -4.618802153516988973, -1.387778780781445676E-14 ) ) ;
#806 = PLANE ( 'NONE',  #7277 ) ;
#807 = DIRECTION ( 'NONE',  ( 0.000000000000000000, 0.000000000000000000, -1.000000000000000000 ) ) ;
#808 = ORIENTED_EDGE ( 'NONE', *, *, #305, .F. ) ;
#809 = DIRECTION ( 'NONE',  ( 0.000000000000000000, 0.000000000000000000, -1.000000000000000000 ) ) ;
#810 = ORIENTED_EDGE ( 'NONE', *, *, #14188, .T. ) ;
#811 = ADVANCED_FACE ( 'NONE', ( #2088 ), #4307, .T. ) ;
#812 = LINE ( 'NONE', #2952, #993 ) ;
#813 = CARTESIAN_POINT ( 'NONE',  ( 0.2174200650117486533, 2.185595227304854227, -3.214438021527926459 ) ) ;
#814 =( LENGTH_UNIT ( ) NAMED_UNIT ( * ) SI_UNIT ( .MILLI., .METRE. ) );
#815 = VERTEX_POINT ( 'NONE', #7418 ) ;
#816 = ORIENTED_EDGE ( 'NONE', *, *, #12022, .T. ) ;
#817 = FACE_OUTER_BOUND ( 'NONE', #5758, .T. ) ;
#818 = DIRECTION ( 'NONE',  ( 0.000000000000000000, 1.000000000000000000, 0.000000000000000000 ) ) ;
#819 = FACE_OUTER_BOUND ( 'NONE', #5661, .T. ) ;
#820 = EDGE_CURVE ( 'NONE', #1356, #9307, #11728, .T. ) ;
#821 = CARTESIAN_POINT ( 'NONE',  ( -5.000000000000004441, 2.886751345948121106, -4.369520038198754897 ) ) ;
#822 = CARTESIAN_POINT ( 'NONE',  ( 0.2174200650117520395, -3.876582599186206846, -0.2855619784720702103 ) ) ;
#823 = DIRECTION ( 'NONE',  ( 0.000000000000000000, 0.000000000000000000, 1.000000000000000000 ) ) ;
#824 = EDGE_CURVE ( 'NONE', #13213, #1861, #709, .T. ) ;
#825 = CARTESIAN_POINT ( 'NONE',  ( 4.093692494532780835, 4.043567292011559289, -1.387813195790392893E-14 ) ) ;
#826 = CARTESIAN_POINT ( 'NONE',  ( 68.68170757442801744, 39.57655509336063915, -117.0000000000000000 ) ) ;
#827 = AXIS2_PLACEMENT_3D ( 'NONE', #1064, #4522, #2445 ) ;
#828 = CARTESIAN_POINT ( 'NONE',  ( 51.90514726928103073, 42.68717498692012668, 25.00000000000000000 ) ) ;
#829 = ORIENTED_EDGE ( 'NONE', *, *, #5080, .F. ) ;
#830 = ORIENTED_EDGE ( 'NONE', *, *, #13086, .T. ) ;
#831 = DIRECTION ( 'NONE',  ( 0.000000000000000000, 0.000000000000000000, -1.000000000000000000 ) ) ;
#832 = DIRECTION ( 'NONE',  ( -1.000000000000000000, 2.551526159633733968E-19, 1.987661601597216239E-18 ) ) ;
#833 = ORIENTED_EDGE ( 'NONE', *, *, #2397, .F. ) ;
#834 = EDGE_CURVE ( 'NONE', #7523, #7727, #8404, .T. ) ;
#835 = CARTESIAN_POINT ( 'NONE',  ( -68.68170757442808849, 39.57655509336051836, 33.00000000000002842 ) ) ;
#836 = ORIENTED_EDGE ( 'NONE', *, *, #571, .T. ) ;
#837 = EDGE_LOOP ( 'NONE', ( #14035, #12060, #7741 ) ) ;
#838 = EDGE_LOOP ( 'NONE', ( #5815, #338, #10885, #914 ) ) ;
#839 = CARTESIAN_POINT ( 'NONE',  ( 31.38313257588132288, 143.6985259526512948, 28.00000000000000000 ) ) ;
#840 = CARTESIAN_POINT ( 'NONE',  ( -3.010143253645307659, 47.91462539009204136, 1.353322078536347339 ) ) ;
#841 = ORIENTED_EDGE ( 'NONE', *, *, #13660, .T. ) ;
#842 = CARTESIAN_POINT ( 'NONE',  ( 5.035982117295204397, -2.314736229921469324, 4.009240756344432555 ) ) ;
#843 = CARTESIAN_POINT ( 'NONE',  ( 76.68170757442798902, 124.5765550933606249, 25.00000000000000000 ) ) ;
#844 = CARTESIAN_POINT ( 'NONE',  ( 20.00000000000000000, 60.00000000000000711, -25.00000000000000000 ) ) ;
#845 = ORIENTED_EDGE ( 'NONE', *, *, #10025, .T. ) ;
#846 = DIRECTION ( 'NONE',  ( 0.000000000000000000, 0.000000000000000000, 1.000000000000000000 ) ) ;
#847 = FACE_OUTER_BOUND ( 'NONE', #5857, .T. ) ;
#848 = DIRECTION ( 'NONE',  ( -1.000000000000000000, 0.000000000000000000, 0.000000000000000000 ) ) ;
#849 = ADVANCED_FACE ( 'NONE', ( #13081 ), #4374, .T. ) ;
#850 = VECTOR ( 'NONE', #2149, 1000.000000000000000 ) ;
#851 = ORIENTED_EDGE ( 'NONE', *, *, #5392, .T. ) ;
#852 = SHAPE_REPRESENTATION ( 'Wedge Roller Guide Pins', ( #11025 ), #12660 ) ;
#853 = ORIENTED_EDGE ( 'NONE', *, *, #2264, .F. ) ;
#854 = ORIENTED_EDGE ( 'NONE', *, *, #1139, .T. ) ;
#855 = CARTESIAN_POINT ( 'NONE',  ( -108.6817075744282448, 109.5765550933602839, 3.299999999999976730 ) ) ;
#856 = ORIENTED_EDGE ( 'NONE', *, *, #10678, .F. ) ;
#857 = DIRECTION ( 'NONE',  ( -0.9240638205168504316, -0.3822382184081046796, 0.000000000000000000 ) ) ;
#858 = DIRECTION ( 'NONE',  ( 1.000000000000000000, 0.000000000000000000, 0.000000000000000000 ) ) ;
#859 = CARTESIAN_POINT ( 'NONE',  ( 3.466359554492712824, 47.71176265719417131, 6.012830585829956220 ) ) ;
#860 = FACE_BOUND ( 'NONE', #711, .T. ) ;
#861 = DIRECTION ( 'NONE',  ( 0.000000000000000000, 0.000000000000000000, -1.000000000000000000 ) ) ;
#862 = APPLICATION_PROTOCOL_DEFINITION ( 'draft international standard', 'automotive_design', 1998, #12047 ) ;
#863 = CARTESIAN_POINT ( 'NONE',  ( 4.101954839143059139, -2.368264730582945177, -3.381130640444254709 ) ) ;
#864 = CARTESIAN_POINT ( 'NONE',  ( 0.000000000000000000, 0.000000000000000000, 25.00000000000000000 ) ) ;
#865 = AXIS2_PLACEMENT_3D ( 'NONE', #12482, #2679, #8292 ) ;
#866 = VECTOR ( 'NONE', #8381, 999.9999999999998863 ) ;
#867 = ADVANCED_FACE ( 'NONE', ( #6458 ), #6254, .F. ) ;
#868 = EDGE_CURVE ( 'NONE', #3118, #5760, #13014, .T. ) ;
#869 = CARTESIAN_POINT ( 'NONE',  ( 19.99999999999999645, 57.00000000000000000, -25.00000000000000000 ) ) ;
#870 = CARTESIAN_POINT ( 'NONE',  ( 76.68170757442804586, -20.42344490663941414, 33.00000000000000000 ) ) ;
#871 = VECTOR ( 'NONE', #14102, 1000.000000000000000 ) ;
#872 = AXIS2_PLACEMENT_3D ( 'NONE', #10007, #2111, #11927 ) ;
#873 = LINE ( 'NONE', #3165, #7989 ) ;
#874 = CARTESIAN_POINT ( 'NONE',  ( 22.00000000000000355, 30.00000000000000711, 25.00000000000000000 ) ) ;
#875 = CARTESIAN_POINT ( 'NONE',  ( 25.00000000000000000, 189.5765550933605539, 47.99999999999998579 ) ) ;
#876 = CARTESIAN_POINT ( 'NONE',  ( 5.005339752383233254, 2.263494164695158961, -4.079513104112302280 ) ) ;
#877 = ORIENTED_EDGE ( 'NONE', *, *, #367, .F. ) ;
#878 = DIRECTION ( 'NONE',  ( 0.000000000000000000, 1.000000000000000000, 0.000000000000000000 ) ) ;
#879 = AXIS2_PLACEMENT_3D ( 'NONE', #5715, #4377, #11362 ) ;
#880 = AXIS2_PLACEMENT_3D ( 'NONE', #8213, #12758, #633 ) ;
#881 = DIRECTION ( 'NONE',  ( 0.000000000000000000, 8.482162385747133845E-47, -1.000000000000000000 ) ) ;
#882 = CARTESIAN_POINT ( 'NONE',  ( 20.00000000000000355, 17.00000000000000000, 25.00000000000000000 ) ) ;
#883 = DIRECTION ( 'NONE',  ( 1.000000000000000000, 0.000000000000000000, 0.000000000000000000 ) ) ;
#884 = CIRCLE ( 'NONE', #1928, 2.500000000000002220 ) ;
#885 = PRODUCT_DEFINITION_CONTEXT ( 'detailed design', #6041, 'design' ) ;
#886 = EDGE_CURVE ( 'NONE', #11486, #7236, #4159, .T. ) ;
#887 = CARTESIAN_POINT ( 'NONE',  ( -1.080113255961760282E-14, -20.42344490663947809, -32.00000000000002842 ) ) ;
#888 = DIRECTION ( 'NONE',  ( 0.000000000000000000, 1.000000000000000000, 0.000000000000000000 ) ) ;
#889 = CYLINDRICAL_SURFACE ( 'NONE', #48, 3.000000000000003553 ) ;
#890 = VECTOR ( 'NONE', #3948, 1000.000000000000000 ) ;
#891 = CONICAL_SURFACE ( 'NONE', #7430, 5.560781378645576645, 1.221730476396047926 ) ;
#892 = FACE_BOUND ( 'NONE', #3702, .T. ) ;
#893 = CARTESIAN_POINT ( 'NONE',  ( 3.333333333333336146, 2.694301256218253116, -3.000726591567075552 ) ) ;
#894 = LINE ( 'NONE', #5363, #5186 ) ;
#895 = ORIENTED_EDGE ( 'NONE', *, *, #5382, .T. ) ;
#896 = CARTESIAN_POINT ( 'NONE',  ( 66.53192852109765454, -5.819950020346492892, 25.00000000000000000 ) ) ;
#897 = CARTESIAN_POINT ( 'NONE',  ( 3.436326524993614129, -2.634838109287991781, -3.231543764078655290 ) ) ;
#898 = EDGE_CURVE ( 'NONE', #5390, #9318, #7561, .T. ) ;
#899 = ORIENTED_EDGE ( 'NONE', *, *, #1154, .F. ) ;
#900 = CARTESIAN_POINT ( 'NONE',  ( 25.00000000000000000, -30.42444490663959300, 47.99999999999998579 ) ) ;
#901 = FACE_BOUND ( 'NONE', #9182, .T. ) ;
#902 = PRESENTATION_LAYER_ASSIGNMENT (  '', '', ( #6742 ) ) ;
#903 = EDGE_LOOP ( 'NONE', ( #2586, #3281, #10639, #10466 ) ) ;
#904 = VERTEX_POINT ( 'NONE', #6329 ) ;
#905 = EDGE_LOOP ( 'NONE', ( #9782, #10029, #10993, #1163 ) ) ;
#906 = DIRECTION ( 'NONE',  ( 0.000000000000000000, 1.000000000000000000, 0.000000000000000000 ) ) ;
#907 = CARTESIAN_POINT ( 'NONE',  ( 108.6817075744280174, 69.57655509336049704, 3.300000000000013589 ) ) ;
#908 = VERTEX_POINT ( 'NONE', #4230 ) ;
#909 = CARTESIAN_POINT ( 'NONE',  ( 3.948103430090711186, -3.379418997638564459, -1.146674596026800330 ) ) ;
#910 = CARTESIAN_POINT ( 'NONE',  ( 5.204170427930318053E-18, -9.648735898059816152E-16, -3.000000000000003553 ) ) ;
#911 = CARTESIAN_POINT ( 'NONE',  ( 61.60657227073433262, 3.881474981106830313, 25.00000000000000000 ) ) ;
#912 = ADVANCED_FACE ( 'NONE', ( #10802 ), #5239, .T. ) ;
#913 = CARTESIAN_POINT ( 'NONE',  ( 20.00000000000000355, 17.00000000000000000, 25.00000000000000000 ) ) ;
#914 = ORIENTED_EDGE ( 'NONE', *, *, #2349, .F. ) ;
#915 = VECTOR ( 'NONE', #4396, 1000.000000000000000 ) ;
#916 = DIRECTION ( 'NONE',  ( 0.000000000000000000, 0.000000000000000000, 1.000000000000000000 ) ) ;
#917 = EDGE_CURVE ( 'NONE', #13885, #9506, #10868, .T. ) ;
#918 = DIRECTION ( 'NONE',  ( -0.9240638205168505426, 0.3822382184081045131, 0.000000000000000000 ) ) ;
#919 = EDGE_LOOP ( 'NONE', ( #5334, #5364 ) ) ;
#920 = ORIENTED_EDGE ( 'NONE', *, *, #12804, .T. ) ;
#921 = ORIENTED_EDGE ( 'NONE', *, *, #4211, .T. ) ;
#922 = VECTOR ( 'NONE', #9203, 1000.000000000000114 ) ;
#923 = PLANE ( 'NONE',  #8498 ) ;
#924 = ORIENTED_EDGE ( 'NONE', *, *, #13227, .T. ) ;
#925 = DIRECTION ( 'NONE',  ( 0.000000000000000000, 1.000000000000000000, 0.000000000000000000 ) ) ;
#926 = CARTESIAN_POINT ( 'NONE',  ( 5.103531824934226080, -2.354098498486466351, -4.077418205400154427 ) ) ;
#927 = CARTESIAN_POINT ( 'NONE',  ( 3.973244831464914029, 47.44383994248515535, 3.467973375954350512 ) ) ;
#928 = EDGE_CURVE ( 'NONE', #2320, #12268, #10145, .T. ) ;
#929 = LINE ( 'NONE', #7732, #11392 ) ;
#930 = DIRECTION ( 'NONE',  ( 1.000000000000000000, 0.000000000000000000, 0.000000000000000000 ) ) ;
#931 = PRODUCT_CONTEXT ( 'NONE', #9027, 'mechanical' ) ;
#932 = CARTESIAN_POINT ( 'NONE',  ( 22.00000000000000355, 40.00000000000000711, 25.00000000000000000 ) ) ;
#933 = CARTESIAN_POINT ( 'NONE',  ( 3.972066048304740082, -2.740530939476243155, 2.384802634787796194 ) ) ;
#934 = CIRCLE ( 'NONE', #1890, 1.500000000000000000 ) ;
#935 = EDGE_LOOP ( 'NONE', ( #9842, #13555 ) ) ;
#936 = EDGE_CURVE ( 'NONE', #1368, #337, #11148, .T. ) ;
#937 = VERTEX_POINT ( 'NONE', #8951 ) ;
#938 = DIRECTION ( 'NONE',  ( 0.000000000000000000, -8.482162385747133845E-47, 1.000000000000000000 ) ) ;
#939 = ORIENTED_EDGE ( 'NONE', *, *, #7348, .T. ) ;
#940 = DIRECTION ( 'NONE',  ( 0.000000000000000000, 0.000000000000000000, -1.000000000000000000 ) ) ;
#941 = VECTOR ( 'NONE', #3510, 1000.000000000000000 ) ;
#942 = ORIENTED_EDGE ( 'NONE', *, *, #10788, .T. ) ;
#943 = PLANE ( 'NONE',  #6123 ) ;
#944 = EDGE_CURVE ( 'NONE', #7467, #1783, #14456, .T. ) ;
#945 = VECTOR ( 'NONE', #3041, 1000.000000000000000 ) ;
#946 = DIRECTION ( 'NONE',  ( -1.000000000000000000, 0.000000000000000000, 0.000000000000000000 ) ) ;
#947 = CARTESIAN_POINT ( 'NONE',  ( 4.859329672868085481, 2.661112198169186982, -3.390818468129665586 ) ) ;
#948 = CARTESIAN_POINT ( 'NONE',  ( 2.000000000000000000, -3.464101615137768153, -2.842992957459220094 ) ) ;
#949 =( NAMED_UNIT ( * ) SI_UNIT ( $, .STERADIAN. ) SOLID_ANGLE_UNIT ( ) );
#950 = VERTEX_POINT ( 'NONE', #13373 ) ;
#951 = ORIENTED_EDGE ( 'NONE', *, *, #8649, .T. ) ;
#952 = CARTESIAN_POINT ( 'NONE',  ( 47.05443476855437268, 62.09002498982675888, 25.00000000000000000 ) ) ;
#953 = CONICAL_SURFACE ( 'NONE', #7496, 2.100000000000000977, 1.029744258676656754 ) ;
#954 = AXIS2_PLACEMENT_3D ( 'NONE', #1864, #9695, #5154 ) ;
#955 = PLANE ( 'NONE',  #5428 ) ;
#956 = DIRECTION ( 'NONE',  ( 1.000000000000000000, 0.000000000000000000, 0.000000000000000000 ) ) ;
#957 = AXIS2_PLACEMENT_3D ( 'NONE', #1843, #13854, #8266 ) ;
#958 = DIRECTION ( 'NONE',  ( 0.000000000000000000, 0.000000000000000000, -1.000000000000000000 ) ) ;
#959 = CARTESIAN_POINT ( 'NONE',  ( 56.99999999999997868, -8.673617379884035472E-16, -25.00000000000000000 ) ) ;
#960 = DIRECTION ( 'NONE',  ( 1.000000000000000000, 0.000000000000000000, -0.000000000000000000 ) ) ;
#961 = DIRECTION ( 'NONE',  ( -1.000000000000000000, -1.665334536937734071E-16, 0.000000000000000000 ) ) ;
#962 = AXIS2_PLACEMENT_3D ( 'NONE', #10682, #11855, #12069 ) ;
#963 = ADVANCED_FACE ( 'NONE', ( #6894 ), #8876, .T. ) ;
#964 = CARTESIAN_POINT ( 'NONE',  ( -997.5739745962155212, 0.000000000000000000, 0.000000000000000000 ) ) ;
#965 = PRESENTATION_LAYER_ASSIGNMENT (  '', '', ( #4032 ) ) ;
#966 = FACE_OUTER_BOUND ( 'NONE', #2432, .T. ) ;
#967 = EDGE_CURVE ( 'NONE', #12483, #10071, #11085, .T. ) ;
#968 =( NAMED_UNIT ( * ) SI_UNIT ( $, .STERADIAN. ) SOLID_ANGLE_UNIT ( ) );
#969 = DIRECTION ( 'NONE',  ( 0.000000000000000000, 0.000000000000000000, -1.000000000000000000 ) ) ;
#970 = EDGE_LOOP ( 'NONE', ( #14106, #13551, #3898, #10691 ) ) ;
#971 = ORIENTED_EDGE ( 'NONE', *, *, #11807, .T. ) ;
#972 = DIRECTION ( 'NONE',  ( 0.000000000000000000, 0.000000000000000000, -1.000000000000000000 ) ) ;
#973 = ADVANCED_FACE ( 'NONE', ( #4450 ), #13506, .F. ) ;
#974 = VERTEX_POINT ( 'NONE', #5712 ) ;
#975 = PLANE ( 'NONE',  #9030 ) ;
#976 = COLOUR_RGB ( '', 0.40784314, 0.44705882, 0.49803922) ;
#977 = LINE ( 'NONE', #3056, #12454 ) ;
#978 = VECTOR ( 'NONE', #140, 1000.000000000000000 ) ;
#979 = AXIS2_PLACEMENT_3D ( 'NONE', #13212, #11893, #4294 ) ;
#980 = ORIENTED_EDGE ( 'NONE', *, *, #12175, .T. ) ;
#981 = VERTEX_POINT ( 'NONE', #3344 ) ;
#982 = CARTESIAN_POINT ( 'NONE',  ( 0.000000000000000000, -4.862606272033103139, -3.445885042887453231 ) ) ;
#983 = LINE ( 'NONE', #4375, #284 ) ;
#984 = DIRECTION ( 'NONE',  ( 0.000000000000000000, 0.000000000000000000, 1.000000000000000000 ) ) ;
#985 = LINE ( 'NONE', #843, #7180 ) ;
#986 = ADVANCED_FACE ( 'NONE', ( #6609 ), #6751, .F. ) ;
#987 = EDGE_CURVE ( 'NONE', #11970, #3878, #9444, .T. ) ;
#988 = CARTESIAN_POINT ( 'NONE',  ( -2.500000000000002220, -1.101719344475953146E-16, -25.03750572909319061 ) ) ;
#989 = PRESENTATION_LAYER_ASSIGNMENT (  '', '', ( #5879 ) ) ;
#990 = CARTESIAN_POINT ( 'NONE',  ( -4.400655246570065238, 3.515428273946862081, -4.476900509771544634 ) ) ;
#991 = AXIS2_PLACEMENT_3D ( 'NONE', #13701, #13850, #10320 ) ;
#992 = VERTEX_POINT ( 'NONE', #4519 ) ;
#993 = VECTOR ( 'NONE', #12897, 999.9999999999998863 ) ;
#994 = FILL_AREA_STYLE_COLOUR ( '', #8422 ) ;
#995 = ADVANCED_FACE ( 'NONE', ( #173 ), #1332, .T. ) ;
#996 = FACE_OUTER_BOUND ( 'NONE', #13697, .T. ) ;
#997 = CARTESIAN_POINT ( 'NONE',  ( 25.00000000000000000, -30.42444490663959300, 47.99999999999998579 ) ) ;
#998 = EDGE_LOOP ( 'NONE', ( #1138, #3336, #3674, #9765 ) ) ;
#999 = EDGE_CURVE ( 'NONE', #9323, #10543, #7783, .T. ) ;
#1000 = VECTOR ( 'NONE', #6749, 1000.000000000000000 ) ;
#1001 = ORIENTED_EDGE ( 'NONE', *, *, #8828, .F. ) ;
#1002 = LINE ( 'NONE', #14406, #5232 ) ;
#1003 = ORIENTED_EDGE ( 'NONE', *, *, #13048, .F. ) ;
#1004 = CARTESIAN_POINT ( 'NONE',  ( 4.033895293470907362, 1.419609371825386823, -3.499999999999992450 ) ) ;
#1005 = ADVANCED_FACE ( 'NONE', ( #1202 ), #4715, .F. ) ;
#1006 = LINE ( 'NONE', #1078, #7921 ) ;
#1007 = EDGE_CURVE ( 'NONE', #8772, #4305, #2374, .T. ) ;
#1008 = LINE ( 'NONE', #8975, #12593 ) ;
#1009 = DIRECTION ( 'NONE',  ( -1.000000000000000000, 0.000000000000000000, 0.000000000000000000 ) ) ;
#1010 = LINE ( 'NONE', #4471, #7742 ) ;
#1011 = ITEM_DEFINED_TRANSFORMATION ( 'NONE', 'NONE', #8500,  #11025 ) ;
#1012 = CARTESIAN_POINT ( 'NONE',  ( 4.154306624731433750, -2.398490048084421122, -3.421999068284433676 ) ) ;
#1013 = CARTESIAN_POINT ( 'NONE',  ( 22.00000000000000000, 80.00000000000000000, -25.00000000000000000 ) ) ;
#1014 = VECTOR ( 'NONE', #5792, 1000.000000000000000 ) ;
#1015 = ADVANCED_FACE ( 'NONE', ( #10127 ), #9015, .F. ) ;
#1016 = VERTEX_POINT ( 'NONE', #13577 ) ;
#1017 = CARTESIAN_POINT ( 'NONE',  ( 4.851472949721049588, 4.233901974057263651, 0.6666666666666831720 ) ) ;
#1018 = AXIS2_PLACEMENT_3D ( 'NONE', #8546, #10822, #12127 ) ;
#1019 = EDGE_LOOP ( 'NONE', ( #1037, #10562, #14464, #7799, #6389 ) ) ;
#1020 = ADVANCED_FACE ( 'NONE', ( #12260 ), #3623, .T. ) ;
#1021 = ADVANCED_FACE ( 'NONE', ( #9987, #11652 ), #1711, .F. ) ;
#1022 = EDGE_LOOP ( 'NONE', ( #14207, #7938, #8866, #13147 ) ) ;
#1023 = PRODUCT_DEFINITION_FORMATION_WITH_SPECIFIED_SOURCE ( 'ANY', '', #10212, .NOT_KNOWN. ) ;
#1024 = ORIENTED_EDGE ( 'NONE', *, *, #3965, .T. ) ;
#1025 =( NAMED_UNIT ( * ) PLANE_ANGLE_UNIT ( ) SI_UNIT ( $, .RADIAN. ) );
#1026 = FACE_OUTER_BOUND ( 'NONE', #13706, .T. ) ;
#1027 = PRESENTATION_STYLE_ASSIGNMENT (( #3166 ) ) ;
#1028 = DIRECTION ( 'NONE',  ( 0.000000000000000000, 0.5000000000000011102, -0.8660254037844379305 ) ) ;
#1029 = ORIENTED_EDGE ( 'NONE', *, *, #14255, .T. ) ;
#1030 = PLANE ( 'NONE',  #1314 ) ;
#1031 = DIRECTION ( 'NONE',  ( -0.5000000000000008882, 0.8660254037844381525, 0.000000000000000000 ) ) ;
#1033 = AXIS2_PLACEMENT_3D ( 'NONE', #242, #7849, #9161 ) ;
#1032 = CARTESIAN_POINT ( 'NONE',  ( 0.000000000000000000, 0.000000000000000000, 0.000000000000000000 ) ) ;
#1034 =( BOUNDED_SURFACE ( )  B_SPLINE_SURFACE ( 3, 2, ( 
 ( #326, #10490, #10644 ),
 ( #550, #8212, #9546 ),
 ( #11660, #8440, #9242 ),
 ( #6084, #5072, #4855 ),
 ( #7037, #472, #12680 ),
 ( #10566, #4789, #6964 ) ),
 .UNSPECIFIED., .F., .F., .F. ) 
 B_SPLINE_SURFACE_WITH_KNOTS ( ( 4, 2, 4 ),
 ( 3, 3 ),
 ( 0.002450104044831662945, 0.005591829551853648266, 0.008733555058875634020 ),
 ( 0.000000000000000000, 1.000000000000000000 ),
 .UNSPECIFIED. ) 
 GEOMETRIC_REPRESENTATION_ITEM ( )  RATIONAL_B_SPLINE_SURFACE ( (
 ( 1.000000000000000000, 0.8047731410850403888, 1.000000000000000000),
 ( 1.000000000000000000, 0.8125552299158879110, 1.000000000000000000),
 ( 1.000000000000000000, 0.8191520442886336406, 1.000000000000000000),
 ( 1.000000000000000000, 0.8191520442893395204, 1.000000000000000000),
 ( 1.000000000000000000, 0.8125552299153580016, 1.000000000000000000),
 ( 1.000000000000000000, 0.8047731410850398337, 1.000000000000000000) ) ) 
 REPRESENTATION_ITEM ( '' )  SURFACE ( )  );
#1035 = CYLINDRICAL_SURFACE ( 'NONE', #14302, 2.100000000000000977 ) ;
#1036 = EDGE_LOOP ( 'NONE', ( #12151, #2448, #6023, #13812 ) ) ;
#1037 = ORIENTED_EDGE ( 'NONE', *, *, #9678, .F. ) ;
#1038 = CARTESIAN_POINT ( 'NONE',  ( 18.68170757442808849, 141.2731697022877313, 35.00000000000000000 ) ) ;
#1039 = CARTESIAN_POINT ( 'NONE',  ( -28.00000000000000355, 24.50000000000001421, 8.000000000000007105 ) ) ;
#1040 = EDGE_CURVE ( 'NONE', #10278, #8394, #11429, .T. ) ;
#1041 = LINE ( 'NONE', #402, #1014 ) ;
#1042 = ADVANCED_BREP_SHAPE_REPRESENTATION ( '', ( #6767, #11025 ), #6359 ) ;
#1043 = CARTESIAN_POINT ( 'NONE',  ( 56.99999999999997868, -8.673617379884035472E-16, 25.00000000000000000 ) ) ;
#1044 = PRODUCT_DEFINITION_CONTEXT ( 'detailed design', #12786, 'design' ) ;
#1045 = CARTESIAN_POINT ( 'NONE',  ( 0.000000000000000000, 0.000000000000000000, -3.500000000000010214 ) ) ;
#1046 = CARTESIAN_POINT ( 'NONE',  ( 22.00000000000000000, 60.00000000000000711, -25.00000000000000000 ) ) ;
#1047 = DIRECTION ( 'NONE',  ( 0.000000000000000000, 0.000000000000000000, 1.000000000000000000 ) ) ;
#1048 = CARTESIAN_POINT ( 'NONE',  ( 2.750000000000003553, 40.49999999999999289, 8.000000000000007105 ) ) ;
#1049 =( NAMED_UNIT ( * ) PLANE_ANGLE_UNIT ( ) SI_UNIT ( $, .RADIAN. ) );
#1050 = CARTESIAN_POINT ( 'NONE',  ( 31.38313257588138683, 143.6985259526510390, -28.00000000000000000 ) ) ;
#1051 = ORIENTED_EDGE ( 'NONE', *, *, #10353, .T. ) ;
#1052 = ORIENTED_EDGE ( 'NONE', *, *, #12586, .T. ) ;
#1053 = CARTESIAN_POINT ( 'NONE',  ( 4.071447262713911996, -2.020725942163681399, -3.500000000000010214 ) ) ;
#1054 = PRESENTATION_STYLE_ASSIGNMENT (( #2158 ) ) ;
#1055 = EDGE_LOOP ( 'NONE', ( #1751, #5944 ) ) ;
#1056 = CARTESIAN_POINT ( 'NONE',  ( 22.00000000000000711, 20.00000000000000355, 25.00000000000000000 ) ) ;
#1057 = EDGE_CURVE ( 'NONE', #8314, #47, #11892, .T. ) ;
#1058 = DIRECTION ( 'NONE',  ( -1.000000000000000000, 0.000000000000000000, 0.000000000000000000 ) ) ;
#1059 = ADVANCED_FACE ( 'NONE', ( #1405 ), #5855, .T. ) ;
#1060 = VERTEX_POINT ( 'NONE', #6163 ) ;
#1061 = DIRECTION ( 'NONE',  ( 0.000000000000000000, 0.000000000000000000, -1.000000000000000000 ) ) ;
#1062 = DIRECTION ( 'NONE',  ( 0.000000000000000000, 0.000000000000000000, 1.000000000000000000 ) ) ;
#1063 = CARTESIAN_POINT ( 'NONE',  ( 3.974175853609971831, -2.726149789692694281, -2.409821656223178454 ) ) ;
#1064 = CARTESIAN_POINT ( 'NONE',  ( 0.000000000000000000, 40.49999999999999289, 8.000000000000007105 ) ) ;
#1065 = CARTESIAN_POINT ( 'NONE',  ( 0.000000000000000000, 0.000000000000000000, 0.000000000000000000 ) ) ;
#1066 = LINE ( 'NONE', #10874, #1839 ) ;
#1067 = ORIENTED_EDGE ( 'NONE', *, *, #2065, .F. ) ;
#1068 = CARTESIAN_POINT ( 'NONE',  ( -2.500000000000011990, 4.330127018922186544, 0.000000000000000000 ) ) ;
#1069 = CYLINDRICAL_SURFACE ( 'NONE', #14439, 5.499999999999980460 ) ;
#1070 = VECTOR ( 'NONE', #4923, 1000.000000000000000 ) ;
#1071 = ORIENTED_EDGE ( 'NONE', *, *, #8262, .T. ) ;
#1072 = EDGE_LOOP ( 'NONE', ( #5271, #2451, #3300, #1091 ) ) ;
#1073 = VERTEX_POINT ( 'NONE', #6075 ) ;
#1074 = LINE ( 'NONE', #9718, #12689 ) ;
#1075 = AXIS2_PLACEMENT_3D ( 'NONE', #6445, #8436, #7403 ) ;
#1076 = EDGE_LOOP ( 'NONE', ( #10467, #5477, #3567, #7124 ) ) ;
#1077 = DIRECTION ( 'NONE',  ( 2.273843122241288438E-18, 5.551115123125782702E-17, 1.000000000000000000 ) ) ;
#1078 = CARTESIAN_POINT ( 'NONE',  ( -8.000000000000000000, 40.49999999999999289, 8.000000000000007105 ) ) ;
#1079 = CARTESIAN_POINT ( 'NONE',  ( 5.599999999999994316, 2.020725942163681399, -3.499999999999996003 ) ) ;
#1080 = CARTESIAN_POINT ( 'NONE',  ( -3.081487911019577365E-30, 3.469446951953614189E-15, -4.900000000000015454 ) ) ;
#1081 = CARTESIAN_POINT ( 'NONE',  ( 57.35294117647057277, -1.411764705882362358, -25.00000000000000000 ) ) ;
#1082 = CARTESIAN_POINT ( 'NONE',  ( 4.197478771013681609, -0.8523759490158168139, -3.205061274276545635 ) ) ;
#1083 = DIRECTION ( 'NONE',  ( -1.000000000000000000, -3.286707217423839940E-17, -2.273843122241288053E-18 ) ) ;
#1084 = VERTEX_POINT ( 'NONE', #12527 ) ;
#1085 = DIRECTION ( 'NONE',  ( 0.000000000000000000, 0.000000000000000000, 1.000000000000000000 ) ) ;
#1086 = ADVANCED_FACE ( 'NONE', ( #2584 ), #10635, .T. ) ;
#1087 = ORIENTED_EDGE ( 'NONE', *, *, #7522, .T. ) ;
#1088 = EDGE_CURVE ( 'NONE', #10667, #12296, #12886, .T. ) ;
#1089 = CARTESIAN_POINT ( 'NONE',  ( 62.10586122665987574, -20.42344490663940704, -28.00000000000000000 ) ) ;
#1090 = ORIENTED_EDGE ( 'NONE', *, *, #9852, .F. ) ;
#1091 = ORIENTED_EDGE ( 'NONE', *, *, #9473, .F. ) ;
#1092 = FILL_AREA_STYLE ('',( #12226 ) ) ;
#1093 = CIRCLE ( 'NONE', #396, 4.000000000000000000 ) ;
#1094 = CARTESIAN_POINT ( 'NONE',  ( 27.57694101601105530, 130.0000000000000000, 25.00000000000000000 ) ) ;
#1095 = CARTESIAN_POINT ( 'NONE',  ( 42.20372226782770753, 81.49287499273339108, 25.00000000000000000 ) ) ;
#1096 = CARTESIAN_POINT ( 'NONE',  ( -129.3408537872145132, 199.5765550933606107, -70.00000000000000000 ) ) ;
#1097 = ORIENTED_EDGE ( 'NONE', *, *, #7571, .T. ) ;
#1098 = LINE ( 'NONE', #5, #8563 ) ;
#1099 = DIRECTION ( 'NONE',  ( 0.000000000000000000, -1.000000000000000000, 0.000000000000000000 ) ) ;
#1100 = CARTESIAN_POINT ( 'NONE',  ( 0.000000000000000000, 0.000000000000000000, 0.000000000000000000 ) ) ;
#1101 = EDGE_CURVE ( 'NONE', #2724, #13213, #13719, .T. ) ;
#1102 = DIRECTION ( 'NONE',  ( 1.000000000000000000, 0.000000000000000000, 0.000000000000000000 ) ) ;
#1103 = VERTEX_POINT ( 'NONE', #9236 ) ;
#1104 = ORIENTED_EDGE ( 'NONE', *, *, #11095, .T. ) ;
#1105 = CARTESIAN_POINT ( 'NONE',  ( -13.00000000000000533, 29.99999999999999289, 8.000000000000007105 ) ) ;
#1106 = CARTESIAN_POINT ( 'NONE',  ( 1.560000000000005826, -1.732050807568885631, 0.000000000000000000 ) ) ;
#1107 = EDGE_CURVE ( 'NONE', #588, #1326, #542, .T. ) ;
#1108 = LINE ( 'NONE', #3244, #10599 ) ;
#1109 = ORIENTED_EDGE ( 'NONE', *, *, #11374, .T. ) ;
#1110 = AXIS2_PLACEMENT_3D ( 'NONE', #10576, #2832, #1800 ) ;
#1111 = VECTOR ( 'NONE', #7469, 1000.000000000000000 ) ;
#1112 = FACE_OUTER_BOUND ( 'NONE', #2519, .T. ) ;
#1113 = DIRECTION ( 'NONE',  ( 0.000000000000000000, 0.000000000000000000, 1.000000000000000000 ) ) ;
#1114 = CARTESIAN_POINT ( 'NONE',  ( 47.05443476855437268, 62.09002498982675888, 25.00000000000000000 ) ) ;
#1115 = LINE ( 'NONE', #6668, #10498 ) ;
#1116 = AXIS2_PLACEMENT_3D ( 'NONE', #1564, #3493, #4656 ) ;
#1117 = EDGE_CURVE ( 'NONE', #12838, #11202, #2635, .T. ) ;
#1118 = CARTESIAN_POINT ( 'NONE',  ( 3.972709601346605890, -3.429395227388305933, -1.191688283765312217 ) ) ;
#1119 = CIRCLE ( 'NONE', #669, 2.100000000000000977 ) ;
#1120 = ORIENTED_EDGE ( 'NONE', *, *, #4565, .T. ) ;
#1121 = CARTESIAN_POINT ( 'NONE',  ( 54.40514726928103784, 42.68717498692012668, 25.00000000000000000 ) ) ;
#1122 =( NAMED_UNIT ( * ) SI_UNIT ( $, .STERADIAN. ) SOLID_ANGLE_UNIT ( ) );
#1123 = VERTEX_POINT ( 'NONE', #13793 ) ;
#1124 = CIRCLE ( 'NONE', #11638, 4.000000000000004441 ) ;
#1125 = LINE ( 'NONE', #8872, #7058 ) ;
#1126 = VECTOR ( 'NONE', #6747, 1000.000000000000000 ) ;
#1127 = AXIS2_PLACEMENT_3D ( 'NONE', #10215, #1359, #3582 ) ;
#1128 = VERTEX_POINT ( 'NONE', #12675 ) ;
#1129 = CARTESIAN_POINT ( 'NONE',  ( 20.00000000000000000, -5.510910596163090344E-15, -25.00000000000000000 ) ) ;
#1130 = DIRECTION ( 'NONE',  ( 1.000000000000000000, 1.224646799147353454E-16, 0.000000000000000000 ) ) ;
#1131 = AXIS2_PLACEMENT_3D ( 'NONE', #7566, #1881, #14324 ) ;
#1132 = DIRECTION ( 'NONE',  ( 0.000000000000000000, 0.000000000000000000, 1.000000000000000000 ) ) ;
#1133 = PLANE ( 'NONE',  #879 ) ;
#1134 =( NAMED_UNIT ( * ) SI_UNIT ( $, .STERADIAN. ) SOLID_ANGLE_UNIT ( ) );
#1135 = LINE ( 'NONE', #3419, #8609 ) ;
#1136 = ADVANCED_FACE ( 'NONE', ( #2736, #623 ), #7033, .F. ) ;
#1137 = DIRECTION ( 'NONE',  ( 0.8191520442889909104, 1.003171929053523637E-16, -0.5735764363510472696 ) ) ;
#1138 = ORIENTED_EDGE ( 'NONE', *, *, #8326, .T. ) ;
#1139 = EDGE_CURVE ( 'NONE', #9318, #5054, #10407, .T. ) ;
#1140 = SURFACE_SIDE_STYLE ('',( #10876 ) ) ;
#1141 = ORIENTED_EDGE ( 'NONE', *, *, #987, .F. ) ;
#1142 = DIRECTION ( 'NONE',  ( -0.9701425001453319874, -0.2425356250363328858, 0.000000000000000000 ) ) ;
#1143 = AXIS2_PLACEMENT_3D ( 'NONE', #11118, #5746, #2 ) ;
#1144 = DIRECTION ( 'NONE',  ( -1.000000000000000000, 0.000000000000000000, 0.000000000000000000 ) ) ;
#1145 = ORIENTED_EDGE ( 'NONE', *, *, #1919, .T. ) ;
#1146 = ORIENTED_EDGE ( 'NONE', *, *, #4200, .T. ) ;
#1147 = EDGE_LOOP ( 'NONE', ( #6680, #4247, #9054, #1407 ) ) ;
#1148 = CARTESIAN_POINT ( 'NONE',  ( 19.99999999999999645, 57.00000000000000000, -25.00000000000000000 ) ) ;
#1149 = ORIENTED_EDGE ( 'NONE', *, *, #1431, .F. ) ;
#1150 = PLANE ( 'NONE',  #3266 ) ;
#1151 = DIRECTION ( 'NONE',  ( 1.000000000000000000, 0.000000000000000000, 0.000000000000000000 ) ) ;
#1152 = EDGE_CURVE ( 'NONE', #12756, #1916, #9781, .T. ) ;
#1153 = CARTESIAN_POINT ( 'NONE',  ( 20.00000000000000000, 60.00000000000000711, 25.00000000000000000 ) ) ;
#1154 = EDGE_CURVE ( 'NONE', #13574, #3245, #13934, .T. ) ;
#1155 = CARTESIAN_POINT ( 'NONE',  ( -3.822382184081044798, 10.25936179483149324, 8.000000000000007105 ) ) ;
#1156 = CARTESIAN_POINT ( 'NONE',  ( 4.000000000000007105, -2.309401076758509141, -3.204271511726779043 ) ) ;
#1157 = CARTESIAN_POINT ( 'NONE',  ( 5.035982117295164429, -4.629472459842958187, -2.775691983046799710E-14 ) ) ;
#1158 = CARTESIAN_POINT ( 'NONE',  ( 4.114405500665259119, -2.025575754679708407, 3.508400121684919881 ) ) ;
#1159 = AXIS2_PLACEMENT_3D ( 'NONE', #13106, #727, #3082 ) ;
#1160 = EDGE_LOOP ( 'NONE', ( #13641, #4625, #1471, #1505 ) ) ;
#1161 = VECTOR ( 'NONE', #2481, 1000.000000000000000 ) ;
#1162 = CARTESIAN_POINT ( 'NONE',  ( 4.000000000000005329, -1.560351142792950174, -0.2242961665059858556 ) ) ;
#1163 = ORIENTED_EDGE ( 'NONE', *, *, #13094, .F. ) ;
#1164 = DIRECTION ( 'NONE',  ( 1.000000000000000000, -2.551526159633733968E-19, -1.987661601597216239E-18 ) ) ;
#1165 = DIRECTION ( 'NONE',  ( 1.000000000000000000, -2.551526159633733968E-19, -1.987661601597216239E-18 ) ) ;
#1166 = CARTESIAN_POINT ( 'NONE',  ( -5.000000000000000888, 2.092595045405802434, -4.400086043326545848 ) ) ;
#1167 = CARTESIAN_POINT ( 'NONE',  ( 1.560000000000005826, -0.8660254037844428154, 1.500000000000001332 ) ) ;
#1168 = ORIENTED_EDGE ( 'NONE', *, *, #4608, .T. ) ;
#1169 = CARTESIAN_POINT ( 'NONE',  ( 22.00000000000000000, 70.00000000000000000, 25.00000000000000000 ) ) ;
#1170 = EDGE_CURVE ( 'NONE', #14055, #6673, #761, .T. ) ;
#1171 = VECTOR ( 'NONE', #2786, 1000.000000000000000 ) ;
#1172 = PLANE ( 'NONE',  #1213 ) ;
#1173 = DIRECTION ( 'NONE',  ( 1.000000000000000000, 0.000000000000000000, 0.000000000000000000 ) ) ;
#1174 = EDGE_CURVE ( 'NONE', #13588, #6553, #10290, .T. ) ;
#1175 = CARTESIAN_POINT ( 'NONE',  ( -4.024497503033517276, 2.323544716729386117, -3.272167766733376393 ) ) ;
#1176 = VERTEX_POINT ( 'NONE', #5217 ) ;
#1177 = CIRCLE ( 'NONE', #713, 3.299999999999997158 ) ;
#1178 = VERTEX_POINT ( 'NONE', #7398 ) ;
#1179 = DIRECTION ( 'NONE',  ( -1.000000000000000000, -0.000000000000000000, -0.000000000000000000 ) ) ;
#1180 = DIRECTION ( 'NONE',  ( 0.000000000000000000, 0.000000000000000000, -1.000000000000000000 ) ) ;
#1181 = VERTEX_POINT ( 'NONE', #11809 ) ;
#1182 = PRESENTATION_LAYER_ASSIGNMENT (  '', '', ( #6068 ) ) ;
#1183 = VECTOR ( 'NONE', #14181, 1000.000000000000000 ) ;
#1184 = FACE_OUTER_BOUND ( 'NONE', #3982, .T. ) ;
#1185 = EDGE_CURVE ( 'NONE', #3592, #433, #14284, .T. ) ;
#1186 = DIRECTION ( 'NONE',  ( 0.000000000000000000, 0.000000000000000000, 1.000000000000000000 ) ) ;
#1187 = CARTESIAN_POINT ( 'NONE',  ( 20.00000000000000000, -5.510910596163090344E-15, -25.00000000000000000 ) ) ;
#1188 = DIRECTION ( 'NONE',  ( -1.000000000000000000, 0.000000000000000000, 0.000000000000000000 ) ) ;
#1189 = EDGE_CURVE ( 'NONE', #3592, #5863, #6306, .T. ) ;
#1190 = VECTOR ( 'NONE', #3310, 1000.000000000000000 ) ;
#1191 = FACE_OUTER_BOUND ( 'NONE', #2416, .T. ) ;
#1192 = ORIENTED_EDGE ( 'NONE', *, *, #2488, .F. ) ;
#1193 = DIRECTION ( 'NONE',  ( -0.000000000000000000, -0.000000000000000000, -1.000000000000000000 ) ) ;
#1194 = VECTOR ( 'NONE', #1542, 1000.000000000000000 ) ;
#1195 = ORIENTED_EDGE ( 'NONE', *, *, #13325, .F. ) ;
#1196 = CARTESIAN_POINT ( 'NONE',  ( 3.384743657228182972E-15, 0.3911686820828953470, 4.000000000000003553 ) ) ;
#1197 = ORIENTED_EDGE ( 'NONE', *, *, #11455, .F. ) ;
#1198 = EDGE_CURVE ( 'NONE', #11002, #6663, #1854, .T. ) ;
#1199 = CIRCLE ( 'NONE', #6095, 2.500000000000002220 ) ;
#1200 =( GEOMETRIC_REPRESENTATION_CONTEXT ( 3 ) GLOBAL_UNCERTAINTY_ASSIGNED_CONTEXT ( ( #2815 ) ) GLOBAL_UNIT_ASSIGNED_CONTEXT ( ( #12457, #5770, #9006 ) ) REPRESENTATION_CONTEXT ( 'NONE', 'WORKASPACE' ) );
#1201 =( GEOMETRIC_REPRESENTATION_CONTEXT ( 3 ) GLOBAL_UNCERTAINTY_ASSIGNED_CONTEXT ( ( #8054 ) ) GLOBAL_UNIT_ASSIGNED_CONTEXT ( ( #10718, #4082, #12760 ) ) REPRESENTATION_CONTEXT ( 'NONE', 'WORKASPACE' ) );
#1202 = FACE_OUTER_BOUND ( 'NONE', #4837, .T. ) ;
#1203 = CARTESIAN_POINT ( 'NONE',  ( 44.70372226782771463, 81.49287499273339108, 25.00000000000000000 ) ) ;
#1204 = DIRECTION ( 'NONE',  ( 0.000000000000000000, 0.000000000000000000, 1.000000000000000000 ) ) ;
#1205 = CARTESIAN_POINT ( 'NONE',  ( 2.750000000000003997, 40.49999999999999289, 0.000000000000000000 ) ) ;
#1206 = CARTESIAN_POINT ( 'NONE',  ( 108.6817075744280459, 189.5765550933606107, 33.00000000000002842 ) ) ;
#1207 = DIRECTION ( 'NONE',  ( 0.000000000000000000, 0.000000000000000000, -1.000000000000000000 ) ) ;
#1208 = ORIENTED_EDGE ( 'NONE', *, *, #13188, .T. ) ;
#1209 = DIRECTION ( 'NONE',  ( 0.000000000000000000, 0.000000000000000000, 1.000000000000000000 ) ) ;
#1210 = VERTEX_POINT ( 'NONE', #11953 ) ;
#1211 = VECTOR ( 'NONE', #13443, 1000.000000000000000 ) ;
#1212 = CARTESIAN_POINT ( 'NONE',  ( 5.599999999999994316, 0.000000000000000000, 0.000000000000000000 ) ) ;
#1213 = AXIS2_PLACEMENT_3D ( 'NONE', #2212, #13258, #3452 ) ;
#1214 = AXIS2_PLACEMENT_3D ( 'NONE', #9472, #13943, #8363 ) ;
#1215 = DIRECTION ( 'NONE',  ( -0.2425356250363330801, 0.9701425001453319874, 0.000000000000000000 ) ) ;
#1216 = EDGE_LOOP ( 'NONE', ( #3549, #605, #13304, #1795 ) ) ;
#1217 = VERTEX_POINT ( 'NONE', #7543 ) ;
#1218 = ADVANCED_FACE ( 'NONE', ( #8573 ), #10705, .T. ) ;
#1219 = VERTEX_POINT ( 'NONE', #3111 ) ;
#1220 = CARTESIAN_POINT ( 'NONE',  ( 22.00000000000000355, 40.00000000000000711, -25.00000000000000000 ) ) ;
#1221 = ORIENTED_EDGE ( 'NONE', *, *, #3777, .T. ) ;
#1222 = CARTESIAN_POINT ( 'NONE',  ( -3.000000000000001332, -1.322063213371143331E-16, 13.31572692736082786 ) ) ;
#1223 = VECTOR ( 'NONE', #11410, 1000.000000000000000 ) ;
#1224 = PRODUCT_DEFINITION_SHAPE ( 'NONE', 'NONE',  #12140 ) ;
#1225 = DIRECTION ( 'NONE',  ( -2.551526159633725302E-19, -1.000000000000000000, 4.440892098500621231E-16 ) ) ;
#1226 = DIRECTION ( 'NONE',  ( 0.000000000000000000, 0.000000000000000000, -1.000000000000000000 ) ) ;
#1227 = CARTESIAN_POINT ( 'NONE',  ( 0.000000000000000000, 17.49899999999995970, 4.000000000000003553 ) ) ;
#1228 = ORIENTED_EDGE ( 'NONE', *, *, #14399, .T. ) ;
#1229 = LINE ( 'NONE', #8834, #12194 ) ;
#1230 = DIRECTION ( 'NONE',  ( 0.9396926207859143121, 1.150791560227857665E-16, -0.3420201433256522816 ) ) ;
#1231 = DIRECTION ( 'NONE',  ( -0.000000000000000000, -0.000000000000000000, -1.000000000000000000 ) ) ;
#1232 =( GEOMETRIC_REPRESENTATION_CONTEXT ( 3 ) GLOBAL_UNCERTAINTY_ASSIGNED_CONTEXT ( ( #9384 ) ) GLOBAL_UNIT_ASSIGNED_CONTEXT ( ( #471, #8358, #629 ) ) REPRESENTATION_CONTEXT ( 'NONE', 'WORKASPACE' ) );
#1233 = CARTESIAN_POINT ( 'NONE',  ( 0.000000000000000000, 0.000000000000000000, 0.000000000000000000 ) ) ;
#1234 = EDGE_LOOP ( 'NONE', ( #7527, #4857, #14209, #14238 ) ) ;
#1235 = EDGE_CURVE ( 'NONE', #14042, #13288, #9119, .T. ) ;
#1236 = EDGE_CURVE ( 'NONE', #14260, #9831, #6440, .T. ) ;
#1237 = CARTESIAN_POINT ( 'NONE',  ( 0.02448804030508137594, 4.877043185438126649, -3.451162025751973950 ) ) ;
#1238 = ORIENTED_EDGE ( 'NONE', *, *, #2251, .T. ) ;
#1239 = CARTESIAN_POINT ( 'NONE',  ( 0.000000000000000000, 0.000000000000000000, 0.000000000000000000 ) ) ;
#1240 = CARTESIAN_POINT ( 'NONE',  ( -2.749999999999997780, 25.49999999999996803, 8.000000000000007105 ) ) ;
#1241 = LINE ( 'NONE', #2558, #4227 ) ;
#1242 = VECTOR ( 'NONE', #3558, 1000.000000000000000 ) ;
#1243 = DIRECTION ( 'NONE',  ( -1.000000000000000000, 0.000000000000000000, 0.000000000000000000 ) ) ;
#1244 = EDGE_CURVE ( 'NONE', #5199, #9008, #14226, .T. ) ;
#1245 = AXIS2_PLACEMENT_3D ( 'NONE', #7766, #7833, #13 ) ;
#1246 = EDGE_LOOP ( 'NONE', ( #2231, #9201, #6977, #5095 ) ) ;
#1247 = DIRECTION ( 'NONE',  ( 0.000000000000000000, 0.000000000000000000, 1.000000000000000000 ) ) ;
#1248 = DIRECTION ( 'NONE',  ( -0.000000000000000000, 1.000000000000000000, -0.000000000000000000 ) ) ;
#1249 = DIRECTION ( 'NONE',  ( -1.000000000000000000, 0.000000000000000000, 0.000000000000000000 ) ) ;
#1250 = DIRECTION ( 'NONE',  ( -1.000000000000000000, 0.000000000000000000, 0.000000000000000000 ) ) ;
#1251 = ORIENTED_EDGE ( 'NONE', *, *, #10457, .T. ) ;
#1252 = VECTOR ( 'NONE', #1971, 1000.000000000000000 ) ;
#1253 = CARTESIAN_POINT ( 'NONE',  ( 22.00000000000000355, 47.00000000000000000, -25.00000000000000000 ) ) ;
#1254 = DIRECTION ( 'NONE',  ( -0.000000000000000000, -8.482162385747133845E-47, 1.000000000000000000 ) ) ;
#1255 = AXIS2_PLACEMENT_3D ( 'NONE', #12234, #6878, #1173 ) ;
#1256 = ORIENTED_EDGE ( 'NONE', *, *, #2632, .F. ) ;
#1257 = VERTEX_POINT ( 'NONE', #4208 ) ;
#1258 = VECTOR ( 'NONE', #5303, 1000.000000000000000 ) ;
#1259 = DIRECTION ( 'NONE',  ( 0.000000000000000000, 0.000000000000000000, 1.000000000000000000 ) ) ;
#1260 = DIRECTION ( 'NONE',  ( -1.000000000000000000, 0.000000000000000000, 0.000000000000000000 ) ) ;
#1261 = LINE ( 'NONE', #10450, #4207 ) ;
#1262 =( NAMED_UNIT ( * ) SI_UNIT ( $, .STERADIAN. ) SOLID_ANGLE_UNIT ( ) );
#1263 = CARTESIAN_POINT ( 'NONE',  ( 4.966173724562063185, -1.610348207484623817, 4.074842637297178882 ) ) ;
#1264 = VERTEX_POINT ( 'NONE', #959 ) ;
#1265 = CARTESIAN_POINT ( 'NONE',  ( -4.203833317240883716, -1.627343821129585422, -3.297273115243907426 ) ) ;
#1266 = EDGE_CURVE ( 'NONE', #9400, #6663, #2842, .T. ) ;
#1267 = VECTOR ( 'NONE', #2666, 1000.000000000000000 ) ;
#1268 = ORIENTED_EDGE ( 'NONE', *, *, #6526, .F. ) ;
#1269 = CARTESIAN_POINT ( 'NONE',  ( 4.175813232069169878, 2.061359961916364725, -3.570380186727395433 ) ) ;
#1270 = EDGE_CURVE ( 'NONE', #10062, #435, #8650, .T. ) ;
#1271 = ADVANCED_FACE ( 'NONE', ( #7464 ), #27, .F. ) ;
#1272 = DIRECTION ( 'NONE',  ( 0.000000000000000000, 0.000000000000000000, 1.000000000000000000 ) ) ;
#1273 = LINE ( 'NONE', #5448, #10327 ) ;
#1274 = CARTESIAN_POINT ( 'NONE',  ( 4.158413352280787123, -2.044871626972824430, -3.541821552872956413 ) ) ;
#1275 = CARTESIAN_POINT ( 'NONE',  ( 42.20372226782770753, 81.49287499273339108, 25.00000000000000000 ) ) ;
#1276 =( LENGTH_UNIT ( ) NAMED_UNIT ( * ) SI_UNIT ( .MILLI., .METRE. ) );
#1277 = CARTESIAN_POINT ( 'NONE',  ( 28.00000000000000355, 29.99999999999999645, 5.738192700042120897 ) ) ;
#1278 = CARTESIAN_POINT ( 'NONE',  ( 53.99999999999997868, -1.324077043022348342E-15, 25.00000000000000000 ) ) ;
#1279 = DIRECTION ( 'NONE',  ( 0.000000000000000000, 0.000000000000000000, -1.000000000000000000 ) ) ;
#1280 = ORIENTED_EDGE ( 'NONE', *, *, #13856, .T. ) ;
#1281 = DIRECTION ( 'NONE',  ( -1.000000000000000000, 0.000000000000000000, 0.000000000000000000 ) ) ;
#1282 = EDGE_CURVE ( 'NONE', #4218, #7189, #7608, .T. ) ;
#1283 = CARTESIAN_POINT ( 'NONE',  ( 1.560000000000005826, 0.8660254037844428154, -1.500000000000001332 ) ) ;
#1284 = ORIENTED_EDGE ( 'NONE', *, *, #12682, .T. ) ;
#1285 =( REPRESENTATION_RELATIONSHIP ('NONE','NONE', #10295, #4961 ) REPRESENTATION_RELATIONSHIP_WITH_TRANSFORMATION ( #1583 )SHAPE_REPRESENTATION_RELATIONSHIP( ) );
#1286 = ORIENTED_EDGE ( 'NONE', *, *, #13904, .T. ) ;
#1287 = CARTESIAN_POINT ( 'NONE',  ( 5.551115123125782702E-14, 1.387778780781445676E-14, -4.000000000000003553 ) ) ;
#1288 = FACE_OUTER_BOUND ( 'NONE', #7499, .T. ) ;
#1289 = CARTESIAN_POINT ( 'NONE',  ( 5.253679160503864409, -3.068491175858450770, -4.666069923292693211 ) ) ;
#1290 = SURFACE_STYLE_FILL_AREA ( #6856 ) ;
#1291 = DIRECTION ( 'NONE',  ( -1.000000000000000000, -3.286707217423839940E-17, -2.273843122241288053E-18 ) ) ;
#1292 = CYLINDRICAL_SURFACE ( 'NONE', #4914, 2.500000000000002220 ) ;
#1293 = ITEM_DEFINED_TRANSFORMATION ( 'NONE', 'NONE', #6623,  #11025 ) ;
#1294 = CARTESIAN_POINT ( 'NONE',  ( 139.9999999999996874, 189.5765550933606107, -132.0000000000000000 ) ) ;
#1296 = AXIS2_PLACEMENT_3D ( 'NONE', #10325, #3832, #2495 ) ;
#1295 = CARTESIAN_POINT ( 'NONE',  ( 1.560000000000005826, 0.000000000000000000, 0.000000000000000000 ) ) ;
#1297 = EDGE_CURVE ( 'NONE', #1257, #9332, #10297, .T. ) ;
#1298 = DIRECTION ( 'NONE',  ( 1.000000000000000000, 0.000000000000000000, 0.000000000000000000 ) ) ;
#1299 = ORIENTED_EDGE ( 'NONE', *, *, #2358, .T. ) ;
#1300 = CARTESIAN_POINT ( 'NONE',  ( 56.68121602037099649, 13.58289998256015352, 25.00000000000000000 ) ) ;
#1301 = CARTESIAN_POINT ( 'NONE',  ( 5.253368672218637236, -3.033033817057797510, -4.659491423763650886 ) ) ;
#1302 = CARTESIAN_POINT ( 'NONE',  ( 4.197393957002307552, 0.8151795401431386479, -3.203767560748919774 ) ) ;
#1303 = DIRECTION ( 'NONE',  ( -1.000000000000000000, -3.286707217423839940E-17, -2.273843122241288053E-18 ) ) ;
#1304 = CARTESIAN_POINT ( 'NONE',  ( 0.3572655899081733644, -4.618802153516988973, -1.387778780781445676E-14 ) ) ;
#1305 = ORIENTED_EDGE ( 'NONE', *, *, #11754, .F. ) ;
#1306 = CARTESIAN_POINT ( 'NONE',  ( 30.15499999999998693, 0.000000000000000000, 0.000000000000000000 ) ) ;
#1307 = EDGE_CURVE ( 'NONE', #10332, #32, #3164, .T. ) ;
#1308 = LINE ( 'NONE', #5757, #1678 ) ;
#1309 = ORIENTED_EDGE ( 'NONE', *, *, #7633, .T. ) ;
#1310 = EDGE_CURVE ( 'NONE', #6345, #11793, #5286, .T. ) ;
#1311 = ORIENTED_EDGE ( 'NONE', *, *, #7811, .F. ) ;
#1312 = DIRECTION ( 'NONE',  ( -0.000000000000000000, -0.000000000000000000, -1.000000000000000000 ) ) ;
#1313 = EDGE_LOOP ( 'NONE', ( #3126, #4583, #612, #8364 ) ) ;
#1314 = AXIS2_PLACEMENT_3D ( 'NONE', #9957, #12301, #13335 ) ;
#1315 = VERTEX_POINT ( 'NONE', #1045 ) ;
#1316 =( BOUNDED_SURFACE ( )  B_SPLINE_SURFACE ( 3, 2, ( 
 ( #6322, #13004, #1867 ),
 ( #2909, #7475, #3125 ),
 ( #14171, #3052, #6451 ),
 ( #10861, #10721, #12039 ),
 ( #10924, #897, #3998 ),
 ( #5367, #8736, #13216 ) ),
 .UNSPECIFIED., .F., .F., .F. ) 
 B_SPLINE_SURFACE_WITH_KNOTS ( ( 4, 2, 4 ),
 ( 3, 3 ),
 ( 0.02023740217035201183, 0.02269762987400600340, 0.02515785757765999150 ),
 ( 0.000000000000000000, 1.000000000000000000 ),
 .UNSPECIFIED. ) 
 GEOMETRIC_REPRESENTATION_ITEM ( )  RATIONAL_B_SPLINE_SURFACE ( (
 ( 1.000000000000000000, 0.8047781539129729156, 1.000000000000000000),
 ( 1.000000000000000000, 0.8123770319059264722, 1.000000000000000000),
 ( 1.000000000000000000, 0.8190663783054025204, 1.000000000000000000),
 ( 1.000000000000000000, 0.8192359702879900007, 1.000000000000000000),
 ( 1.000000000000000000, 0.8126134888417688718, 1.000000000000000000),
 ( 1.000000000000000000, 0.8047712368238112424, 1.000000000000000000) ) ) 
 REPRESENTATION_ITEM ( '' )  SURFACE ( )  );
#1317 = UNCERTAINTY_MEASURE_WITH_UNIT (LENGTH_MEASURE( 1.000000000000000082E-05 ), #6135, 'distance_accuracy_value', 'NONE');
#1318 = CARTESIAN_POINT ( 'NONE',  ( 4.851472949721049588, 4.233901974057263651, -0.6666666666666535290 ) ) ;
#1319 = DIRECTION ( 'NONE',  ( 0.000000000000000000, 1.000000000000000000, -0.000000000000000000 ) ) ;
#1320 = VERTEX_POINT ( 'NONE', #5501 ) ;
#1321 = ORIENTED_EDGE ( 'NONE', *, *, #3326, .F. ) ;
#1322 = CARTESIAN_POINT ( 'NONE',  ( 22.00000000000000000, 60.00000000000000711, 25.00000000000000000 ) ) ;
#1323 = VECTOR ( 'NONE', #124, 1000.000000000000000 ) ;
#1324 = CARTESIAN_POINT ( 'NONE',  ( 118.6817075744280316, 109.5765550933604828, 0.000000000000000000 ) ) ;
#1325 = VECTOR ( 'NONE', #14394, 1000.000000000000000 ) ;
#1326 = VERTEX_POINT ( 'NONE', #2147 ) ;
#1327 = CARTESIAN_POINT ( 'NONE',  ( 20.00000000000000000, -5.510910596163090344E-15, -25.00000000000000000 ) ) ;
#1328 = VERTEX_POINT ( 'NONE', #7687 ) ;
#1329 = PRODUCT_DEFINITION_SHAPE ( 'NONE', 'NONE',  #14473 ) ;
#1330 = EDGE_LOOP ( 'NONE', ( #14150, #4446, #3501, #2087, #3645, #980, #2647, #10197 ) ) ;
#1331 = UNCERTAINTY_MEASURE_WITH_UNIT (LENGTH_MEASURE( 1.000000000000000082E-05 ), #10231, 'distance_accuracy_value', 'NONE');
#1332 = PLANE ( 'NONE',  #12478 ) ;
#1333 = CARTESIAN_POINT ( 'NONE',  ( 5.103531824934115946, -2.354098498486438373, 4.077418205400141105 ) ) ;
#1334 = AXIS2_PLACEMENT_3D ( 'NONE', #3699, #6904, #10418 ) ;
#1335 = EDGE_LOOP ( 'NONE', ( #7967, #9486, #2581, #7234, #12217, #11618, #7087 ) ) ;
#1336 = AXIS2_PLACEMENT_3D ( 'NONE', #10596, #6410, #11911 ) ;
#1337 = CARTESIAN_POINT ( 'NONE',  ( 2.369999999999996998, 5.817072295949927426E-16, -4.750000000000000000 ) ) ;
#1338 = CARTESIAN_POINT ( 'NONE',  ( 0.000000000000000000, 17.49899999999995970, 8.000000000000003553 ) ) ;
#1339 = CARTESIAN_POINT ( 'NONE',  ( 6.938893903907228378E-15, 24.50000000000002132, 8.000000000000007105 ) ) ;
#1340 = LINE ( 'NONE', #3421, #10474 ) ;
#1341 = VERTEX_POINT ( 'NONE', #11070 ) ;
#1342 = DIRECTION ( 'NONE',  ( -1.000000000000000000, -1.927470528863119049E-16, 0.000000000000000000 ) ) ;
#1343 = EDGE_CURVE ( 'NONE', #6304, #2703, #7663, .T. ) ;
#1344 = VERTEX_POINT ( 'NONE', #12164 ) ;
#1345 = CARTESIAN_POINT ( 'NONE',  ( -4.999999999999999112, 1.924500897298744517, -4.118275046351175916 ) ) ;
#1346 = DIRECTION ( 'NONE',  ( 0.000000000000000000, 0.000000000000000000, 1.000000000000000000 ) ) ;
#1347 = ORIENTED_EDGE ( 'NONE', *, *, #10810, .F. ) ;
#1348 = FACE_OUTER_BOUND ( 'NONE', #13937, .T. ) ;
#1349 = AXIS2_PLACEMENT_3D ( 'NONE', #1038, #4350, #9963 ) ;
#1350 = VERTEX_POINT ( 'NONE', #8149 ) ;
#1351 = AXIS2_PLACEMENT_3D ( 'NONE', #12401, #11364, #7926 ) ;
#1352 = VERTEX_POINT ( 'NONE', #9484 ) ;
#1353 = CARTESIAN_POINT ( 'NONE',  ( 1.560000000000005826, 0.000000000000000000, -1.500000000000001332 ) ) ;
#1354 = CARTESIAN_POINT ( 'NONE',  ( 8.178185494084536283E-16, 3.857556137907083293, -1.318516776095773224 ) ) ;
#1355 = ADVANCED_FACE ( 'NONE', ( #8074 ), #11466, .T. ) ;
#1356 = VERTEX_POINT ( 'NONE', #1506 ) ;
#1357 = PLANE ( 'NONE',  #13573 ) ;
#1358 = LINE ( 'NONE', #5804, #6464 ) ;
#1359 = DIRECTION ( 'NONE',  ( -0.000000000000000000, 1.000000000000000000, 0.000000000000000000 ) ) ;
#1360 = AXIS2_PLACEMENT_3D ( 'NONE', #49, #11157, #14398 ) ;
#1361 = PLANE ( 'NONE',  #11448 ) ;
#1362 = CONTEXT_DEPENDENT_SHAPE_REPRESENTATION ( #13266, #12947 ) ;
#1363 = EDGE_CURVE ( 'NONE', #25, #4424, #4943, .T. ) ;
#1364 = CARTESIAN_POINT ( 'NONE',  ( 3.951447005078475350, 2.357513599190963927, 2.916666666666662078 ) ) ;
#1365 = CARTESIAN_POINT ( 'NONE',  ( -129.3408537872145132, 189.5765550933606107, -70.00000000000000000 ) ) ;
#1366 = DIRECTION ( 'NONE',  ( -1.000000000000000000, 0.000000000000000000, 0.000000000000000000 ) ) ;
#1367 = VECTOR ( 'NONE', #13668, 1000.000000000000000 ) ;
#1368 = VERTEX_POINT ( 'NONE', #11670 ) ;
#1369 = CARTESIAN_POINT ( 'NONE',  ( -0.6641139335926458109, 4.471067008845417412, -3.302142222888703849 ) ) ;
#1370 = ORIENTED_EDGE ( 'NONE', *, *, #11562, .T. ) ;
#1371 = EDGE_CURVE ( 'NONE', #6548, #8214, #1905, .T. ) ;
#1372 = DIRECTION ( 'NONE',  ( 1.000000000000000000, 3.286707217423839940E-17, 2.273843122241288053E-18 ) ) ;
#1373 = AXIS2_PLACEMENT_3D ( 'NONE', #5187, #4969, #7375 ) ;
#1374 = LINE ( 'NONE', #9204, #8230 ) ;
#1375 = CARTESIAN_POINT ( 'NONE',  ( -5.000000000000000000, 1.069517409952100095, -4.273100593733644814 ) ) ;
#1376 = CARTESIAN_POINT ( 'NONE',  ( 58.68170757442803165, 29.57655509336062849, -33.00000000000000000 ) ) ;
#1377 = VERTEX_POINT ( 'NONE', #1649 ) ;
#1378 = LINE ( 'NONE', #10313, #262 ) ;
#1379 = DIRECTION ( 'NONE',  ( 0.000000000000000000, 0.000000000000000000, -1.000000000000000000 ) ) ;
#1380 = DIRECTION ( 'NONE',  ( 0.000000000000000000, 1.000000000000000000, 0.000000000000000000 ) ) ;
#1381 = EDGE_CURVE ( 'NONE', #1103, #1315, #4919, .T. ) ;
#1382 = MECHANICAL_DESIGN_GEOMETRIC_PRESENTATION_REPRESENTATION (  '', ( #3971 ), #9336 ) ;
#1383 = CARTESIAN_POINT ( 'NONE',  ( 22.00000000000000711, 20.00000000000000355, 25.00000000000000000 ) ) ;
#1384 = STYLED_ITEM ( 'NONE', ( #1027 ), #1904 ) ;
#1385 = ORIENTED_EDGE ( 'NONE', *, *, #13324, .T. ) ;
#1386 = EDGE_LOOP ( 'NONE', ( #10991, #9939, #6561, #8171 ) ) ;
#1387 = EDGE_CURVE ( 'NONE', #5595, #313, #12174, .T. ) ;
#1388 = EDGE_LOOP ( 'NONE', ( #2561, #11617, #939, #10546 ) ) ;
#1389 = AXIS2_PLACEMENT_3D ( 'NONE', #2479, #13763, #7222 ) ;
#1390 = CARTESIAN_POINT ( 'NONE',  ( -2.171643655288370667, 3.365003104552331870, -7.639672495602285140E-15 ) ) ;
#1391 = LINE ( 'NONE', #7911, #1671 ) ;
#1392 =( NAMED_UNIT ( * ) PLANE_ANGLE_UNIT ( ) SI_UNIT ( $, .RADIAN. ) );
#1393 = VERTEX_POINT ( 'NONE', #9403 ) ;
#1394 = ORIENTED_EDGE ( 'NONE', *, *, #679, .F. ) ;
#1395 = CYLINDRICAL_SURFACE ( 'NONE', #5325, 8.000000000000000000 ) ;
#1396 = VECTOR ( 'NONE', #6858, 1000.000000000000000 ) ;
#1397 = LINE ( 'NONE', #2579, #11974 ) ;
#1398 = AXIS2_PLACEMENT_3D ( 'NONE', #8081, #3866, #8300 ) ;
#1399 = ORIENTED_EDGE ( 'NONE', *, *, #6270, .T. ) ;
#1400 = SHAPE_REPRESENTATION ( 'bushing', ( #11025 ), #4496 ) ;
#1401 = CARTESIAN_POINT ( 'NONE',  ( 20.00000000000000000, 80.00000000000000000, -25.00000000000000000 ) ) ;
#1402 = ORIENTED_EDGE ( 'NONE', *, *, #2494, .T. ) ;
#1403 = ADVANCED_FACE ( 'NONE', ( #12851 ), #8223, .F. ) ;
#1404 = EDGE_CURVE ( 'NONE', #6344, #11164, #11446, .T. ) ;
#1405 = FACE_OUTER_BOUND ( 'NONE', #10834, .T. ) ;
#1406 = CARTESIAN_POINT ( 'NONE',  ( 4.142654963991843076, 2.035398498734334538, 3.525413613457302198 ) ) ;
#1407 = ORIENTED_EDGE ( 'NONE', *, *, #10352, .T. ) ;
#1408 = AXIS2_PLACEMENT_3D ( 'NONE', #4546, #5891, #4746 ) ;
#1409 = DIRECTION ( 'NONE',  ( 0.000000000000000000, 0.000000000000000000, 1.000000000000000000 ) ) ;
#1410 = VECTOR ( 'NONE', #8000, 1000.000000000000000 ) ;
#1411 = CARTESIAN_POINT ( 'NONE',  ( 0.000000000000000000, 0.000000000000000000, 0.000000000000000000 ) ) ;
#1412 = CARTESIAN_POINT ( 'NONE',  ( 0.000000000000000000, 0.000000000000000000, -4.674599999999973221 ) ) ;
#1413 = CARTESIAN_POINT ( 'NONE',  ( 4.871660775260050258, 3.916561903058253691, 1.361048636879866658 ) ) ;
#1414 = AXIS2_PLACEMENT_3D ( 'NONE', #6975, #339, #10579 ) ;
#1415 = EDGE_CURVE ( 'NONE', #10068, #5462, #7017, .T. ) ;
#1416 = ORIENTED_EDGE ( 'NONE', *, *, #13645, .F. ) ;
#1417 = CARTESIAN_POINT ( 'NONE',  ( -140.0000000000003411, 189.5765550933606107, 47.99999999999998579 ) ) ;
#1418 = B_SPLINE_CURVE_WITH_KNOTS ( 'NONE', 3,
 ( #3045, #5146, #11813, #546, #6237 ),
 .UNSPECIFIED., .F., .F.,
 ( 4, 1, 4 ),
 ( 0.000000000000000000, 0.002886751345948135056, 0.005773502691896269245 ),
 .UNSPECIFIED. ) ;
#1419 = ORIENTED_EDGE ( 'NONE', *, *, #11341, .T. ) ;
#1420 = CARTESIAN_POINT ( 'NONE',  ( 3.000000000000000888, 3.469446951953614189E-15, -6.000000000000005329 ) ) ;
#1421 = CARTESIAN_POINT ( 'NONE',  ( 21.68170757442808849, 141.2731697022877313, 35.00000000000000000 ) ) ;
#1422 = EDGE_LOOP ( 'NONE', ( #3931, #617 ) ) ;
#1423 = LINE ( 'NONE', #1283, #5753 ) ;
#1424 = AXIS2_PLACEMENT_3D ( 'NONE', #12440, #8035, #12508 ) ;
#1425 = AXIS2_PLACEMENT_3D ( 'NONE', #7083, #3889, #12576 ) ;
#1426 = ORIENTED_EDGE ( 'NONE', *, *, #3621, .T. ) ;
#1427 = CARTESIAN_POINT ( 'NONE',  ( 5.013196232911400152, 4.621129290018668456, -2.362106518389725739E-18 ) ) ;
#1428 = ORIENTED_EDGE ( 'NONE', *, *, #12406, .T. ) ;
#1429 = EDGE_CURVE ( 'NONE', #9259, #815, #12695, .T. ) ;
#1430 = ORIENTED_EDGE ( 'NONE', *, *, #6494, .T. ) ;
#1431 = EDGE_CURVE ( 'NONE', #4518, #7883, #10070, .T. ) ;
#1432 = DIRECTION ( 'NONE',  ( -1.000000000000000000, -8.619211990076296383E-16, 0.000000000000000000 ) ) ;
#1433 = CARTESIAN_POINT ( 'NONE',  ( 118.6817075744280316, 109.5765550933604828, 0.000000000000000000 ) ) ;
#1434 = ORIENTED_EDGE ( 'NONE', *, *, #7156, .T. ) ;
#1435 = CARTESIAN_POINT ( 'NONE',  ( -5.000000000000000000, -0.4954705650270034845, 7.301424005332068923E-16 ) ) ;
#1436 = CARTESIAN_POINT ( 'NONE',  ( 20.00000000000000000, -5.510910596163090344E-15, -25.00000000000000000 ) ) ;
#1437 = VECTOR ( 'NONE', #9792, 1000.000000000000000 ) ;
#1438 = LINE ( 'NONE', #7875, #11643 ) ;
#1439 = AXIS2_PLACEMENT_3D ( 'NONE', #11177, #2196, #10158 ) ;
#1440 = CIRCLE ( 'NONE', #3797, 5.499999999999975131 ) ;
#1441 = CARTESIAN_POINT ( 'NONE',  ( 0.000000000000000000, 40.49999999999999289, 8.000000000000007105 ) ) ;
#1442 = FACE_OUTER_BOUND ( 'NONE', #10048, .T. ) ;
#1443 = CARTESIAN_POINT ( 'NONE',  ( 0.3572655899081733644, 2.309401076758504701, -3.999999999999989786 ) ) ;
#1444 = DIRECTION ( 'NONE',  ( 0.000000000000000000, 1.000000000000000000, 0.000000000000000000 ) ) ;
#1445 = EDGE_CURVE ( 'NONE', #8503, #8261, #12465, .T. ) ;
#1446 = ADVANCED_FACE ( 'NONE', ( #10505 ), #13953, .T. ) ;
#1447 = ORIENTED_EDGE ( 'NONE', *, *, #2115, .T. ) ;
#1448 = VECTOR ( 'NONE', #12943, 1000.000000000000000 ) ;
#1449 = AXIS2_PLACEMENT_3D ( 'NONE', #4221, #13074, #9757 ) ;
#1450 = CIRCLE ( 'NONE', #10572, 1.500000000000000000 ) ;
#1451 = CIRCLE ( 'NONE', #3083, 3.299999999999969624 ) ;
#1452 = ORIENTED_EDGE ( 'NONE', *, *, #11500, .F. ) ;
#1453 = EDGE_CURVE ( 'NONE', #7600, #3428, #1733, .T. ) ;
#1454 = ADVANCED_FACE ( 'NONE', ( #3639, #2066 ), #8789, .T. ) ;
#1455 = ORIENTED_EDGE ( 'NONE', *, *, #13368, .T. ) ;
#1456 = CARTESIAN_POINT ( 'NONE',  ( -28.00000000000000355, 29.99999999999999645, 8.000000000000007105 ) ) ;
#1457 = CARTESIAN_POINT ( 'NONE',  ( 37.27836601746437850, 91.19429999418670718, 25.00000000000000000 ) ) ;
#1458 = CARTESIAN_POINT ( 'NONE',  ( -5.000000000000000000, 1.088034370075782409, -4.020973883015756201 ) ) ;
#1459 = ADVANCED_FACE ( 'NONE', ( #12163 ), #10983, .T. ) ;
#1460 = LINE ( 'NONE', #3520, #8902 ) ;
#1461 = CARTESIAN_POINT ( 'NONE',  ( 13.00000000000000533, 35.49999999999997158, 0.000000000000000000 ) ) ;
#1462 = DIRECTION ( 'NONE',  ( 0.000000000000000000, 0.000000000000000000, -1.000000000000000000 ) ) ;
#1463 =( GEOMETRIC_REPRESENTATION_CONTEXT ( 3 ) GLOBAL_UNCERTAINTY_ASSIGNED_CONTEXT ( ( #12594 ) ) GLOBAL_UNIT_ASSIGNED_CONTEXT ( ( #1937, #9751, #3116 ) ) REPRESENTATION_CONTEXT ( 'NONE', 'WORKASPACE' ) );
#1464 = PLANE ( 'NONE',  #12425 ) ;
#1465 = CIRCLE ( 'NONE', #308, 2.749999999999997780 ) ;
#1466 = AXIS2_PLACEMENT_3D ( 'NONE', #11474, #5689, #295 ) ;
#1467 = PRODUCT_DEFINITION_SHAPE ( 'NONE', 'NONE',  #13858 ) ;
#1468 = B_SPLINE_CURVE_WITH_KNOTS ( 'NONE', 3,
 ( #1515, #14045, #12705, #11836, #1580 ),
 .UNSPECIFIED., .F., .F.,
 ( 4, 1, 4 ),
 ( 0.000000000000000000, 0.002886751345948134623, 0.005773502691896269245 ),
 .UNSPECIFIED. ) ;
#1469 = EDGE_CURVE ( 'NONE', #3034, #3917, #16, .T. ) ;
#1470 = LINE ( 'NONE', #8188, #12661 ) ;
#1471 = ORIENTED_EDGE ( 'NONE', *, *, #8427, .F. ) ;
#1472 = ORIENTED_EDGE ( 'NONE', *, *, #10760, .F. ) ;
#1473 = AXIS2_PLACEMENT_3D ( 'NONE', #14275, #4336, #8771 ) ;
#1474 = DIRECTION ( 'NONE',  ( 1.000000000000000000, 0.000000000000000000, -0.000000000000000000 ) ) ;
#1475 = LINE ( 'NONE', #2572, #5846 ) ;
#1476 = SURFACE_STYLE_USAGE ( .BOTH. , #6223 ) ;
#1477 = VERTEX_POINT ( 'NONE', #13348 ) ;
#1478 =( REPRESENTATION_RELATIONSHIP ('NONE','NONE', #10295, #8802 ) REPRESENTATION_RELATIONSHIP_WITH_TRANSFORMATION ( #3219 )SHAPE_REPRESENTATION_RELATIONSHIP( ) );
#1479 = ORIENTED_EDGE ( 'NONE', *, *, #1749, .F. ) ;
#1480 = FACE_OUTER_BOUND ( 'NONE', #4601, .T. ) ;
#1481 = ADVANCED_FACE ( 'NONE', ( #1112 ), #5566, .T. ) ;
#1482 = CIRCLE ( 'NONE', #2415, 2.499999999999999556 ) ;
#1483 = LINE ( 'NONE', #11353, #14080 ) ;
#1484 = VERTEX_POINT ( 'NONE', #11203 ) ;
#1485 = DIRECTION ( 'NONE',  ( 0.000000000000000000, 0.000000000000000000, -1.000000000000000000 ) ) ;
#1486 = CONICAL_SURFACE ( 'NONE', #7542, 2.100000000000000977, 1.029744258676656754 ) ;
#1487 = ORIENTED_EDGE ( 'NONE', *, *, #12210, .T. ) ;
#1488 = UNCERTAINTY_MEASURE_WITH_UNIT (LENGTH_MEASURE( 1.000000000000000082E-05 ), #9973, 'distance_accuracy_value', 'NONE');
#1489 = DIRECTION ( 'NONE',  ( -1.000000000000000000, 0.000000000000000000, 0.000000000000000000 ) ) ;
#1490 = PLANE ( 'NONE',  #4984 ) ;
#1491 = AXIS2_PLACEMENT_3D ( 'NONE', #10614, #8402, #7150 ) ;
#1492 = CARTESIAN_POINT ( 'NONE',  ( 108.6817075744280174, 109.5765550933605113, 1.102182119232617753E-14 ) ) ;
#1493 = CARTESIAN_POINT ( 'NONE',  ( 5.005210506770622736, 2.400510894617556623, -4.000000000000002665 ) ) ;
#1494 = FACE_OUTER_BOUND ( 'NONE', #3379, .T. ) ;
#1495 = CARTESIAN_POINT ( 'NONE',  ( 2.369999999999996998, 0.000000000000000000, 0.000000000000000000 ) ) ;
#1496 = ORIENTED_EDGE ( 'NONE', *, *, #3852, .F. ) ;
#1497 = AXIS2_PLACEMENT_3D ( 'NONE', #1574, #6026, #7203 ) ;
#1498 = CARTESIAN_POINT ( 'NONE',  ( -5.000000000000003553, -1.924500897298772939, -4.118275046351175028 ) ) ;
#1499 = ADVANCED_FACE ( 'NONE', ( #1184 ), #8661, .T. ) ;
#1500 = EDGE_CURVE ( 'NONE', #144, #904, #9130, .T. ) ;
#1501 = CARTESIAN_POINT ( 'NONE',  ( 1.390214784104953027, 4.043996922316329901, -3.202509183706280460 ) ) ;
#1502 = ORIENTED_EDGE ( 'NONE', *, *, #3655, .T. ) ;
#1503 = FACE_OUTER_BOUND ( 'NONE', #6913, .T. ) ;
#1504 = CARTESIAN_POINT ( 'NONE',  ( 5.103531824934115946, -2.354098498486438373, 4.077418205400141105 ) ) ;
#1505 = ORIENTED_EDGE ( 'NONE', *, *, #12501, .F. ) ;
#1506 = CARTESIAN_POINT ( 'NONE',  ( 0.000000000000000000, -4.862606272033103139, -3.445885042887453231 ) ) ;
#1507 = VERTEX_POINT ( 'NONE', #7353 ) ;
#1508 = ORIENTED_EDGE ( 'NONE', *, *, #9688, .F. ) ;
#1509 = ORIENTED_EDGE ( 'NONE', *, *, #9134, .T. ) ;
#1510 = DIRECTION ( 'NONE',  ( 1.000000000000000000, 0.000000000000000000, -0.000000000000000000 ) ) ;
#1511 = CARTESIAN_POINT ( 'NONE',  ( -2.450325270861127613, 48.11882021490243488, 7.172319002129952992 ) ) ;
#1512 = AXIS2_PLACEMENT_3D ( 'NONE', #4552, #6998, #4613 ) ;
#1513 = ORIENTED_EDGE ( 'NONE', *, *, #2251, .F. ) ;
#1514 = CARTESIAN_POINT ( 'NONE',  ( 0.000000000000000000, 0.000000000000000000, -3.500000000000010214 ) ) ;
#1515 = CARTESIAN_POINT ( 'NONE',  ( -5.000000000000001776, -2.886751345948152192, -4.284345921091780696 ) ) ;
#1516 = LINE ( 'NONE', #5029, #199 ) ;
#1517 = DIRECTION ( 'NONE',  ( 0.000000000000000000, 0.000000000000000000, 1.000000000000000000 ) ) ;
#1518 = FILL_AREA_STYLE ('',( #12707 ) ) ;
#1519 = PLANE ( 'NONE',  #4004 ) ;
#1520 = DIRECTION ( 'NONE',  ( 1.000000000000000000, 0.000000000000000000, 0.000000000000000000 ) ) ;
#1521 = CARTESIAN_POINT ( 'NONE',  ( 4.082498951862935321, 2.020725942163680511, -3.499999999999997780 ) ) ;
#1522 = LINE ( 'NONE', #10104, #2529 ) ;
#1523 = VERTEX_POINT ( 'NONE', #14370 ) ;
#1524 = CARTESIAN_POINT ( 'NONE',  ( 4.101954839143062692, 2.368264730582934519, -3.381130640444258262 ) ) ;
#1525 = VERTEX_POINT ( 'NONE', #11830 ) ;
#1526 = ORIENTED_EDGE ( 'NONE', *, *, #58, .F. ) ;
#1527 = DIRECTION ( 'NONE',  ( -0.2425356250363328581, 0.9701425001453318764, 0.000000000000000000 ) ) ;
#1528 = CARTESIAN_POINT ( 'NONE',  ( 0.000000000000000000, -3.031088913245536087, 1.750000000000001554 ) ) ;
#1529 = DIRECTION ( 'NONE',  ( 1.000000000000000000, 1.665334536937734071E-16, 0.000000000000000000 ) ) ;
#1530 = LINE ( 'NONE', #11553, #8631 ) ;
#1531 = LINE ( 'NONE', #10681, #1666 ) ;
#1532 = CARTESIAN_POINT ( 'NONE',  ( 51.90514726928103073, 42.68717498692012668, 25.00000000000000000 ) ) ;
#1533 = CARTESIAN_POINT ( 'NONE',  ( 4.175813232069169878, -4.122719923832743660, -6.938893903907228378E-15 ) ) ;
#1534 = CARTESIAN_POINT ( 'NONE',  ( 1.317756351988342622, -3.857995168970220767, -0.04852650426603082046 ) ) ;
#1535 = EDGE_CURVE ( 'NONE', #11633, #13672, #6590, .T. ) ;
#1536 = CARTESIAN_POINT ( 'NONE',  ( -118.6817075744282306, 109.5765550933602839, 3.299999999999983391 ) ) ;
#1537 = EDGE_LOOP ( 'NONE', ( #12834, #4232, #7012, #1145 ) ) ;
#1538 = EDGE_LOOP ( 'NONE', ( #4094, #2861 ) ) ;
#1539 = ORIENTED_EDGE ( 'NONE', *, *, #4420, .F. ) ;
#1540 = ORIENTED_EDGE ( 'NONE', *, *, #4596, .F. ) ;
#1541 = DIRECTION ( 'NONE',  ( 1.000000000000000000, 1.913084959030911013E-15, 0.000000000000000000 ) ) ;
#1542 = DIRECTION ( 'NONE',  ( 0.000000000000000000, 0.000000000000000000, 1.000000000000000000 ) ) ;
#1543 = ADVANCED_FACE ( 'NONE', ( #11133 ), #11023, .F. ) ;
#1544 = FILL_AREA_STYLE ('',( #13860 ) ) ;
#1545 = VERTEX_POINT ( 'NONE', #1043 ) ;
#1546 = EDGE_CURVE ( 'NONE', #1084, #8394, #9968, .T. ) ;
#1547 = ORIENTED_EDGE ( 'NONE', *, *, #6614, .T. ) ;
#1548 = DIRECTION ( 'NONE',  ( 0.000000000000000000, 0.000000000000000000, 1.000000000000000000 ) ) ;
#1549 = PLANE ( 'NONE',  #5866 ) ;
#1550 = AXIS2_PLACEMENT_3D ( 'NONE', #152, #7897, #11269 ) ;
#1551 = VERTEX_POINT ( 'NONE', #13204 ) ;
#1552 = DIRECTION ( 'NONE',  ( -1.000000000000000000, 0.000000000000000000, 0.000000000000000000 ) ) ;
#1553 = DIRECTION ( 'NONE',  ( 0.000000000000000000, 1.000000000000000000, 0.000000000000000000 ) ) ;
#1554 = LINE ( 'NONE', #11653, #1070 ) ;
#1555 = EDGE_CURVE ( 'NONE', #8738, #12036, #8933, .T. ) ;
#1556 = CYLINDRICAL_SURFACE ( 'NONE', #13817, 3.299999999999997158 ) ;
#1557 = CARTESIAN_POINT ( 'NONE',  ( 20.00000000000000000, 60.00000000000000711, 25.00000000000000000 ) ) ;
#1558 =( NAMED_UNIT ( * ) SI_UNIT ( $, .STERADIAN. ) SOLID_ANGLE_UNIT ( ) );
#1559 = DIRECTION ( 'NONE',  ( 0.000000000000000000, 0.000000000000000000, 1.000000000000000000 ) ) ;
#1560 = DIRECTION ( 'NONE',  ( 0.000000000000000000, 0.000000000000000000, 1.000000000000000000 ) ) ;
#1561 = ORIENTED_EDGE ( 'NONE', *, *, #14170, .T. ) ;
#1562 = CARTESIAN_POINT ( 'NONE',  ( 0.3126073911696169993, 2.020725942163681399, -3.499999999999996003 ) ) ;
#1563 = VERTEX_POINT ( 'NONE', #6738 ) ;
#1565 = EDGE_CURVE ( 'NONE', #5395, #6157, #7605, .T. ) ;
#1564 = CARTESIAN_POINT ( 'NONE',  ( -108.6817075744281595, 69.57655509336026967, 0.000000000000000000 ) ) ;
#1566 = CARTESIAN_POINT ( 'NONE',  ( 3.472352378023054520, 2.614038573344155125, -3.020318136128903319 ) ) ;
#1567 = ORIENTED_EDGE ( 'NONE', *, *, #556, .T. ) ;
#1568 = CARTESIAN_POINT ( 'NONE',  ( 5.085139881807307916, -4.657383176246346679, 0.06682429157518411655 ) ) ;
#1569 = FACE_BOUND ( 'NONE', #11379, .T. ) ;
#1570 = EDGE_LOOP ( 'NONE', ( #11826, #4173, #11309, #4560 ) ) ;
#1571 = CARTESIAN_POINT ( 'NONE',  ( 28.00000000000000355, 29.99999999999999645, 0.000000000000000000 ) ) ;
#1572 = EDGE_LOOP ( 'NONE', ( #7051, #8246 ) ) ;
#1573 = VERTEX_POINT ( 'NONE', #12516 ) ;
#1574 = CARTESIAN_POINT ( 'NONE',  ( 22.00000000000000355, 50.00000000000000000, -25.00000000000000000 ) ) ;
#1575 = CARTESIAN_POINT ( 'NONE',  ( 139.9999999999996874, 199.5765550933606107, 47.99999999999998579 ) ) ;
#1576 = ADVANCED_FACE ( 'NONE', ( #4836 ), #8046, .T. ) ;
#1577 = VERTEX_POINT ( 'NONE', #9147 ) ;
#1578 = CARTESIAN_POINT ( 'NONE',  ( 3.679171394226034231, 2.494631558665835858, -0.3503314178412536006 ) ) ;
#1579 = EDGE_CURVE ( 'NONE', #1934, #3640, #10326, .T. ) ;
#1580 = CARTESIAN_POINT ( 'NONE',  ( -1.752700365193367750E-15, -5.773502691896304384, -4.284345921091780696 ) ) ;
#1581 = FACE_OUTER_BOUND ( 'NONE', #504, .T. ) ;
#1582 = DIRECTION ( 'NONE',  ( -1.000000000000000000, 0.000000000000000000, 0.000000000000000000 ) ) ;
#1583 = ITEM_DEFINED_TRANSFORMATION ( 'NONE', 'NONE', #8966,  #11025 ) ;
#1584 = DIRECTION ( 'NONE',  ( -1.321694076934709169E-16, 1.000000000000000000, -0.000000000000000000 ) ) ;
#1585 = CARTESIAN_POINT ( 'NONE',  ( 0.000000000000000000, 0.000000000000000000, 0.000000000000000000 ) ) ;
#1586 = FACE_OUTER_BOUND ( 'NONE', #7438, .T. ) ;
#1587 = AXIS2_PLACEMENT_3D ( 'NONE', #581, #9640, #10739 ) ;
#1588 = CARTESIAN_POINT ( 'NONE',  ( 0.000000000000000000, 4.862606272033096033, -3.445885042887453231 ) ) ;
#1589 = CIRCLE ( 'NONE', #11877, 5.499999999999980460 ) ;
#1590 = EDGE_LOOP ( 'NONE', ( #13097, #7525, #7860, #7717 ) ) ;
#1591 = CARTESIAN_POINT ( 'NONE',  ( 4.024499207728662320, 2.323545700935577329, -3.272172305156505701 ) ) ;
#1592 = ORIENTED_EDGE ( 'NONE', *, *, #11567, .F. ) ;
#1593 = EDGE_CURVE ( 'NONE', #5280, #11750, #9299, .T. ) ;
#1594 = VERTEX_POINT ( 'NONE', #6951 ) ;
#1595 = AXIS2_PLACEMENT_3D ( 'NONE', #2769, #12950, #6194 ) ;
#1596 = DIRECTION ( 'NONE',  ( -1.000000000000000000, 0.000000000000000000, -0.000000000000000000 ) ) ;
#1597 = DIRECTION ( 'NONE',  ( 1.734723475976770694E-18, -4.440892098500621231E-16, -1.000000000000000000 ) ) ;
#1598 = CARTESIAN_POINT ( 'NONE',  ( 20.00000000000000000, 47.00000000000000000, 25.00000000000000000 ) ) ;
#1599 = AXIS2_PLACEMENT_3D ( 'NONE', #5171, #7423, #11909 ) ;
#1600 = CARTESIAN_POINT ( 'NONE',  ( 19.99999999999999645, 67.00000000000000000, 25.00000000000000000 ) ) ;
#1601 = CARTESIAN_POINT ( 'NONE',  ( 5.067058822021066611, -2.325541950156887694, -4.027956812804548647 ) ) ;
#1602 = FACE_OUTER_BOUND ( 'NONE', #12063, .T. ) ;
#1603 = APPLICATION_PROTOCOL_DEFINITION ( 'draft international standard', 'automotive_design', 1998, #4579 ) ;
#1604 = DIRECTION ( 'NONE',  ( 0.000000000000000000, -8.482162385747133845E-47, 1.000000000000000000 ) ) ;
#1605 = CARTESIAN_POINT ( 'NONE',  ( 20.00000000000000355, 30.00000000000000711, 25.00000000000000000 ) ) ;
#1606 = EDGE_CURVE ( 'NONE', #1393, #8011, #1475, .T. ) ;
#1607 = VECTOR ( 'NONE', #8017, 1000.000000000000000 ) ;
#1608 = CARTESIAN_POINT ( 'NONE',  ( 4.379424050594069584, 3.527728022193128865, -4.490801088233107308 ) ) ;
#1609 = ORIENTED_EDGE ( 'NONE', *, *, #9227, .F. ) ;
#1610 = ORIENTED_EDGE ( 'NONE', *, *, #2488, .T. ) ;
#1611 = EDGE_CURVE ( 'NONE', #1181, #588, #7961, .T. ) ;
#1612 = EDGE_CURVE ( 'NONE', #11488, #1123, #160, .T. ) ;
#1613 = FACE_OUTER_BOUND ( 'NONE', #5829, .T. ) ;
#1614 = PLANE ( 'NONE',  #3089 ) ;
#1615 = CIRCLE ( 'NONE', #7686, 2.054999999999999716 ) ;
#1616 =( NAMED_UNIT ( * ) SI_UNIT ( $, .STERADIAN. ) SOLID_ANGLE_UNIT ( ) );
#1617 = EDGE_CURVE ( 'NONE', #6928, #8393, #1391, .T. ) ;
#1618 = EDGE_LOOP ( 'NONE', ( #12820, #14405, #5969 ) ) ;
#1619 = VECTOR ( 'NONE', #9205, 1000.000000000000000 ) ;
#1620 = LINE ( 'NONE', #14009, #6263 ) ;
#1621 = CARTESIAN_POINT ( 'NONE',  ( 0.000000000000000000, 3.061616997868382155E-16, -2.499999999999999112 ) ) ;
#1622 = ADVANCED_FACE ( 'NONE', ( #7977 ), #11348, .T. ) ;
#1623 = ORIENTED_EDGE ( 'NONE', *, *, #14426, .T. ) ;
#1624 = EDGE_CURVE ( 'NONE', #7658, #7309, #5463, .T. ) ;
#1625 = CARTESIAN_POINT ( 'NONE',  ( -5.000000000000001776, -2.886751345948152192, -4.369520038198755785 ) ) ;
#1626 = VECTOR ( 'NONE', #3990, 1000.000000000000000 ) ;
#1627 = ORIENTED_EDGE ( 'NONE', *, *, #13810, .T. ) ;
#1628 = UNCERTAINTY_MEASURE_WITH_UNIT (LENGTH_MEASURE( 1.000000000000000082E-05 ), #6520, 'distance_accuracy_value', 'NONE');
#1629 = ADVANCED_FACE ( 'NONE', ( #6815 ), #12659, .F. ) ;
#1630 = DIRECTION ( 'NONE',  ( 1.000000000000000000, 1.665334536937734071E-16, 0.000000000000000000 ) ) ;
#1631 = CARTESIAN_POINT ( 'NONE',  ( 4.872568031907682951, -3.922980182067751898, 1.349977486297343043 ) ) ;
#1632 = CARTESIAN_POINT ( 'NONE',  ( 5.000000000000001776, 2.886751345948127767, -6.000000000000005329 ) ) ;
#1633 = ADVANCED_FACE ( 'NONE', ( #7019 ), #2652, .T. ) ;
#1634 = ORIENTED_EDGE ( 'NONE', *, *, #6804, .T. ) ;
#1635 = DIRECTION ( 'NONE',  ( -0.9240638205168504316, -0.3822382184081046796, 0.000000000000000000 ) ) ;
#1636 = DIRECTION ( 'NONE',  ( 0.000000000000000000, -1.000000000000000000, -0.000000000000000000 ) ) ;
#1637 = ORIENTED_EDGE ( 'NONE', *, *, #13104, .T. ) ;
#1638 = DIRECTION ( 'NONE',  ( -1.000000000000000000, 0.000000000000000000, 0.000000000000000000 ) ) ;
#1639 = CARTESIAN_POINT ( 'NONE',  ( 36.99999999999999289, 80.00000000000000000, -25.00000000000000000 ) ) ;
#1640 = LINE ( 'NONE', #6011, #3763 ) ;
#1641 = AXIS2_PLACEMENT_3D ( 'NONE', #5730, #345, #9335 ) ;
#1642 = ADVANCED_FACE ( 'NONE', ( #5702 ), #9843, .T. ) ;
#1643 = DIRECTION ( 'NONE',  ( 0.000000000000000000, 1.000000000000000000, 0.000000000000000000 ) ) ;
#1644 = DIRECTION ( 'NONE',  ( 1.000000000000000000, 0.000000000000000000, 0.000000000000000000 ) ) ;
#1645 = VERTEX_POINT ( 'NONE', #8115 ) ;
#1646 = LINE ( 'NONE', #778, #12787 ) ;
#1647 = EDGE_CURVE ( 'NONE', #9523, #181, #102, .T. ) ;
#1648 = FACE_BOUND ( 'NONE', #6730, .T. ) ;
#1649 = CARTESIAN_POINT ( 'NONE',  ( 22.28098402457126426, 141.4229888148237535, 33.00000000000000000 ) ) ;
#1650 = ORIENTED_EDGE ( 'NONE', *, *, #2508, .F. ) ;
#1651 = MECHANICAL_DESIGN_GEOMETRIC_PRESENTATION_REPRESENTATION (  '', ( #14280 ), #3532 ) ;
#1652 = ORIENTED_EDGE ( 'NONE', *, *, #12936, .T. ) ;
#1653 = AXIS2_PLACEMENT_3D ( 'NONE', #964, #8726, #8862 ) ;
#1654 = LINE ( 'NONE', #12854, #2675 ) ;
#1655 = CARTESIAN_POINT ( 'NONE',  ( 22.00000000000000000, 70.00000000000000000, 25.00000000000000000 ) ) ;
#1656 = EDGE_LOOP ( 'NONE', ( #4322, #4081, #13598, #12074 ) ) ;
#1657 = DIRECTION ( 'NONE',  ( 1.000000000000000000, 0.000000000000000000, 0.000000000000000000 ) ) ;
#1658 = CARTESIAN_POINT ( 'NONE',  ( 22.00000000000000355, 47.00000000000000000, -25.00000000000000000 ) ) ;
#1659 = SURFACE_SIDE_STYLE ('',( #417 ) ) ;
#1660 = AXIS2_PLACEMENT_3D ( 'NONE', #13162, #6050, #12116 ) ;
#1661 = LINE ( 'NONE', #6109, #10008 ) ;
#1662 = ORIENTED_EDGE ( 'NONE', *, *, #820, .T. ) ;
#1663 = CARTESIAN_POINT ( 'NONE',  ( 0.000000000000000000, 0.000000000000000000, 0.000000000000000000 ) ) ;
#1664 = CARTESIAN_POINT ( 'NONE',  ( 95.04167153547044222, -149.6197612287760705, 33.00000000000000000 ) ) ;
#1665 = DIRECTION ( 'NONE',  ( 0.000000000000000000, 5.551115123125782702E-17, 1.000000000000000000 ) ) ;
#1666 = VECTOR ( 'NONE', #5975, 1000.000000000000000 ) ;
#1667 = FACE_BOUND ( 'NONE', #4349, .T. ) ;
#1668 = AXIS2_PLACEMENT_3D ( 'NONE', #1417, #2595, #7041 ) ;
#1669 = CARTESIAN_POINT ( 'NONE',  ( 76.68170757442804586, -20.42344490663941414, -33.00000000000000000 ) ) ;
#1670 = EDGE_CURVE ( 'NONE', #408, #8822, #268, .T. ) ;
#1671 = VECTOR ( 'NONE', #310, 1000.000000000000000 ) ;
#1672 = ORIENTED_EDGE ( 'NONE', *, *, #3743, .T. ) ;
#1673 = CARTESIAN_POINT ( 'NONE',  ( 40.00000000000000711, 80.00000000000000000, 25.00000000000000000 ) ) ;
#1674 = EDGE_LOOP ( 'NONE', ( #6926, #2420, #5165, #9689 ) ) ;
#1675 = ORIENTED_EDGE ( 'NONE', *, *, #10881, .F. ) ;
#1676 = LINE ( 'NONE', #2631, #9345 ) ;
#1677 = MECHANICAL_DESIGN_GEOMETRIC_PRESENTATION_REPRESENTATION (  '', ( #4032 ), #3781 ) ;
#1678 = VECTOR ( 'NONE', #13260, 1000.000000000000000 ) ;
#1679 = LINE ( 'NONE', #7224, #8428 ) ;
#1680 = CARTESIAN_POINT ( 'NONE',  ( 22.00000000000000000, 70.00000000000000000, 25.00000000000000000 ) ) ;
#1681 = DIRECTION ( 'NONE',  ( 0.000000000000000000, 0.000000000000000000, -1.000000000000000000 ) ) ;
#1682 = CARTESIAN_POINT ( 'NONE',  ( 5.035982117295206173, -2.314736229921483535, -4.009240756344418344 ) ) ;
#1683 = PLANE ( 'NONE',  #4495 ) ;
#1684 = CARTESIAN_POINT ( 'NONE',  ( 0.000000000000000000, 0.000000000000000000, 0.000000000000000000 ) ) ;
#1685 = LINE ( 'NONE', #10684, #5641 ) ;
#1686 = LINE ( 'NONE', #602, #7972 ) ;
#1687 = VECTOR ( 'NONE', #1130, 1000.000000000000000 ) ;
#1688 = EDGE_CURVE ( 'NONE', #3669, #13670, #9002, .T. ) ;
#1689 = VECTOR ( 'NONE', #13552, 1000.000000000000000 ) ;
#1690 = CIRCLE ( 'NONE', #2874, 4.750000000000000000 ) ;
#1691 = ADVANCED_FACE ( 'NONE', ( #13566 ), #3537, .F. ) ;
#1692 = CARTESIAN_POINT ( 'NONE',  ( 0.000000000000000000, 0.000000000000000000, 13.31572692736082786 ) ) ;
#1693 = VERTEX_POINT ( 'NONE', #6222 ) ;
#1694 = ORIENTED_EDGE ( 'NONE', *, *, #9360, .T. ) ;
#1695 = ORIENTED_EDGE ( 'NONE', *, *, #1670, .F. ) ;
#1696 = EDGE_CURVE ( 'NONE', #10936, #1577, #14075, .T. ) ;
#1697 = LINE ( 'NONE', #10547, #5430 ) ;
#1698 = CARTESIAN_POINT ( 'NONE',  ( -4.024497503033519052, -2.323544716729397219, -3.272167766733379946 ) ) ;
#1699 = COLOUR_RGB ( '', 0.72549020, 0.75294118, 0.79215686) ;
#1700 = CIRCLE ( 'NONE', #7988, 2.500000000000002220 ) ;
#1701 = AXIS2_PLACEMENT_3D ( 'NONE', #13476, #10899, #2207 ) ;
#1702 = VERTEX_POINT ( 'NONE', #11867 ) ;
#1703 = ORIENTED_EDGE ( 'NONE', *, *, #2205, .F. ) ;
#1704 = LINE ( 'NONE', #14151, #10227 ) ;
#1705 = DIRECTION ( 'NONE',  ( 2.133709875451472726E-16, -1.000000000000000000, -0.000000000000000000 ) ) ;
#1706 = ORIENTED_EDGE ( 'NONE', *, *, #4939, .F. ) ;
#1707 = DIRECTION ( 'NONE',  ( 1.000000000000000000, 1.665334536937733825E-16, 0.000000000000000000 ) ) ;
#1708 = VECTOR ( 'NONE', #2266, 1000.000000000000000 ) ;
#1709 = PRODUCT ( 'Hardened Serrated Safety Wedge', 'Hardened Serrated Safety Wedge', '', ( #3087 ) ) ;
#1710 = ORIENTED_EDGE ( 'NONE', *, *, #5542, .T. ) ;
#1711 = PLANE ( 'NONE',  #10377 ) ;
#1712 = CARTESIAN_POINT ( 'NONE',  ( 5.238704763094644612, 1.015773027556919228, -4.385839086323478853 ) ) ;
#1713 = CARTESIAN_POINT ( 'NONE',  ( 30.60000000000001563, 0.000000000000000000, 0.000000000000000000 ) ) ;
#1714 = ORIENTED_EDGE ( 'NONE', *, *, #6615, .T. ) ;
#1715 = CARTESIAN_POINT ( 'NONE',  ( 4.175326769692884632, 4.121399112977849555, -8.369832099842142803E-15 ) ) ;
#1716 = CARTESIAN_POINT ( 'NONE',  ( 56.99999999999997868, -8.673617379884035472E-16, 23.00000000000000000 ) ) ;
#1717 = SURFACE_STYLE_FILL_AREA ( #13940 ) ;
#1718 = EDGE_LOOP ( 'NONE', ( #3786, #2990 ) ) ;
#1719 = DIRECTION ( 'NONE',  ( 0.000000000000000000, 0.000000000000000000, 1.000000000000000000 ) ) ;
#1720 = DIRECTION ( 'NONE',  ( 0.000000000000000000, 0.000000000000000000, 1.000000000000000000 ) ) ;
#1721 = AXIS2_PLACEMENT_3D ( 'NONE', #688, #4065, #2281 ) ;
#1722 = VERTEX_POINT ( 'NONE', #12984 ) ;
#1723 = CARTESIAN_POINT ( 'NONE',  ( 22.00000000000000000, 70.00000000000000000, 25.00000000000000000 ) ) ;
#1724 = DIRECTION ( 'NONE',  ( 0.000000000000000000, 0.000000000000000000, 1.000000000000000000 ) ) ;
#1725 = PLANE ( 'NONE',  #4726 ) ;
#1726 = VECTOR ( 'NONE', #12961, 1000.000000000000000 ) ;
#1727 = EDGE_CURVE ( 'NONE', #8738, #13954, #7266, .T. ) ;
#1728 = ORIENTED_EDGE ( 'NONE', *, *, #13993, .T. ) ;
#1729 = LINE ( 'NONE', #7412, #13044 ) ;
#1730 = EDGE_CURVE ( 'NONE', #12256, #3727, #4276, .T. ) ;
#1731 = CARTESIAN_POINT ( 'NONE',  ( -4.000000000000000888, -1.539600717839011423, -3.000726591567076884 ) ) ;
#1732 = AXIS2_PLACEMENT_3D ( 'NONE', #13699, #6938, #9288 ) ;
#1733 = LINE ( 'NONE', #10655, #7488 ) ;
#1734 = ORIENTED_EDGE ( 'NONE', *, *, #1758, .F. ) ;
#1735 = ORIENTED_EDGE ( 'NONE', *, *, #13842, .F. ) ;
#1736 = DIRECTION ( 'NONE',  ( 0.000000000000000000, 0.000000000000000000, 1.000000000000000000 ) ) ;
#1737 = FACE_OUTER_BOUND ( 'NONE', #5106, .T. ) ;
#1738 = VERTEX_POINT ( 'NONE', #2953 ) ;
#1739 = CARTESIAN_POINT ( 'NONE',  ( 33.99999999999998579, 80.00000000000000000, 23.00000000000000000 ) ) ;
#1740 = VECTOR ( 'NONE', #9766, 1000.000000000000114 ) ;
#1741 = CARTESIAN_POINT ( 'NONE',  ( 4.960860176462274396, 1.574785417369866769, 4.074727069546279168 ) ) ;
#1742 = CARTESIAN_POINT ( 'NONE',  ( 54.35294117647056567, -1.411764705882362358, 25.00000000000000000 ) ) ;
#1743 = EDGE_CURVE ( 'NONE', #4861, #4373, #3896, .T. ) ;
#1744 = CARTESIAN_POINT ( 'NONE',  ( -13.00000000000000533, 35.49999999999997158, 0.000000000000000000 ) ) ;
#1745 = EDGE_LOOP ( 'NONE', ( #6476, #4758, #12311, #5613 ) ) ;
#1746 =( LENGTH_UNIT ( ) NAMED_UNIT ( * ) SI_UNIT ( .MILLI., .METRE. ) );
#1747 = DIRECTION ( 'NONE',  ( 1.000000000000000000, -0.000000000000000000, -0.000000000000000000 ) ) ;
#1748 = DIRECTION ( 'NONE',  ( 0.000000000000000000, 0.000000000000000000, -1.000000000000000000 ) ) ;
#1749 = EDGE_CURVE ( 'NONE', #6344, #12541, #746, .T. ) ;
#1750 = CARTESIAN_POINT ( 'NONE',  ( 1.144235203016672475, 3.958177651039092471, -0.09382832055445862462 ) ) ;
#1751 = ORIENTED_EDGE ( 'NONE', *, *, #13733, .F. ) ;
#1752 = LINE ( 'NONE', #6125, #2421 ) ;
#1753 = VERTEX_POINT ( 'NONE', #14148 ) ;
#1754 = ORIENTED_EDGE ( 'NONE', *, *, #3468, .T. ) ;
#1755 = CARTESIAN_POINT ( 'NONE',  ( 22.00000000000000711, 20.00000000000000355, -25.00000000000000000 ) ) ;
#1756 = DIRECTION ( 'NONE',  ( -1.000000000000000000, 2.551526159633733968E-19, 1.987661601597216239E-18 ) ) ;
#1757 = CARTESIAN_POINT ( 'NONE',  ( 1.051966859446179514, 48.43488408057972805, 0.1316037626694079310 ) ) ;
#1758 = EDGE_CURVE ( 'NONE', #10181, #11306, #2144, .T. ) ;
#1759 = DIRECTION ( 'NONE',  ( -0.000000000000000000, 1.000000000000000000, -0.000000000000000000 ) ) ;
#1760 = DIRECTION ( 'NONE',  ( 0.000000000000000000, -8.482162385747133845E-47, 1.000000000000000000 ) ) ;
#1761 = APPLICATION_PROTOCOL_DEFINITION ( 'draft international standard', 'automotive_design', 1998, #8089 ) ;
#1762 = CARTESIAN_POINT ( 'NONE',  ( -4.204015924366186319, 1.626724848190924000, -3.310627190413372389 ) ) ;
#1763 = CARTESIAN_POINT ( 'NONE',  ( 4.033901012034863065, -3.740908793663352938, 0.5205559028927786436 ) ) ;
#1764 = ORIENTED_EDGE ( 'NONE', *, *, #163, .T. ) ;
#1765 = ADVANCED_FACE ( 'NONE', ( #2727, #3030 ), #1614, .T. ) ;
#1766 = CARTESIAN_POINT ( 'NONE',  ( 0.1391502195351279059, -2.687187980154724265, -3.345653888883624028 ) ) ;
#1767 = VERTEX_POINT ( 'NONE', #4988 ) ;
#1768 = ORIENTED_EDGE ( 'NONE', *, *, #2005, .T. ) ;
#1769 = ORIENTED_EDGE ( 'NONE', *, *, #8326, .F. ) ;
#1770 = CIRCLE ( 'NONE', #11106, 2.750000000000003553 ) ;
#1771 =( REPRESENTATION_RELATIONSHIP ('NONE','NONE', #10295, #3865 ) REPRESENTATION_RELATIONSHIP_WITH_TRANSFORMATION ( #5889 )SHAPE_REPRESENTATION_RELATIONSHIP( ) );
#1772 = VERTEX_POINT ( 'NONE', #1774 ) ;
#1773 = DIRECTION ( 'NONE',  ( -1.000000000000000000, 0.000000000000000000, 0.000000000000000000 ) ) ;
#1774 = CARTESIAN_POINT ( 'NONE',  ( 20.00000000000000000, 5.000000000000000000, 25.00000000000000000 ) ) ;
#1775 = EDGE_CURVE ( 'NONE', #9307, #7122, #7738, .T. ) ;
#1776 = EDGE_CURVE ( 'NONE', #5852, #7349, #11238, .T. ) ;
#1777 = VERTEX_POINT ( 'NONE', #5126 ) ;
#1778 = CARTESIAN_POINT ( 'NONE',  ( 5.284804376168109386, -3.015249596956831368, -4.666192694417973463 ) ) ;
#1779 = VECTOR ( 'NONE', #960, 1000.000000000000000 ) ;
#1780 = CARTESIAN_POINT ( 'NONE',  ( 78.52142056027061301, -86.08568224108226730, 28.00000000000000000 ) ) ;
#1781 = VERTEX_POINT ( 'NONE', #10624 ) ;
#1782 = CARTESIAN_POINT ( 'NONE',  ( 4.175813232069169878, -4.122719923832743660, -6.938893903907228378E-15 ) ) ;
#1783 = VERTEX_POINT ( 'NONE', #7388 ) ;
#1784 = UNCERTAINTY_MEASURE_WITH_UNIT (LENGTH_MEASURE( 1.000000000000000082E-05 ), #2241, 'distance_accuracy_value', 'NONE');
#1785 = DIRECTION ( 'NONE',  ( 0.000000000000000000, -1.000000000000000000, 0.000000000000000000 ) ) ;
#1786 = CARTESIAN_POINT ( 'NONE',  ( 44.70372226782771463, 81.49287499273339108, -25.00000000000000000 ) ) ;
#1787 = DIRECTION ( 'NONE',  ( 0.000000000000000000, -8.482162385747133845E-47, 1.000000000000000000 ) ) ;
#1788 = VERTEX_POINT ( 'NONE', #12898 ) ;
#1789 = CARTESIAN_POINT ( 'NONE',  ( 21.68170757442808849, 141.2731697022877313, -35.00000000000000000 ) ) ;
#1790 = DIRECTION ( 'NONE',  ( 1.000000000000000000, 0.000000000000000000, -0.000000000000000000 ) ) ;
#1791 =( LENGTH_UNIT ( ) NAMED_UNIT ( * ) SI_UNIT ( .MILLI., .METRE. ) );
#1792 = ORIENTED_EDGE ( 'NONE', *, *, #12682, .F. ) ;
#1793 = CARTESIAN_POINT ( 'NONE',  ( 57.35294117647057277, -1.411764705882362358, -25.00000000000000000 ) ) ;
#1794 = DIRECTION ( 'NONE',  ( 0.000000000000000000, 0.000000000000000000, 1.000000000000000000 ) ) ;
#1795 = ORIENTED_EDGE ( 'NONE', *, *, #3657, .T. ) ;
#1796 = LINE ( 'NONE', #2827, #10774 ) ;
#1797 = DIRECTION ( 'NONE',  ( 1.665334536937734071E-16, -1.000000000000000000, 0.000000000000000000 ) ) ;
#1798 = LINE ( 'NONE', #11825, #7044 ) ;
#1799 = ORIENTED_EDGE ( 'NONE', *, *, #9028, .F. ) ;
#1800 = DIRECTION ( 'NONE',  ( 1.000000000000000000, 1.665334536937734071E-16, 0.000000000000000000 ) ) ;
#1801 = FACE_OUTER_BOUND ( 'NONE', #11405, .T. ) ;
#1802 = ORIENTED_EDGE ( 'NONE', *, *, #10042, .T. ) ;
#1803 = EDGE_LOOP ( 'NONE', ( #8409, #10422, #4006 ) ) ;
#1804 = CARTESIAN_POINT ( 'NONE',  ( 22.00000000000000000, 67.00000000000000000, -25.00000000000000000 ) ) ;
#1805 = CARTESIAN_POINT ( 'NONE',  ( -3.466359554492713269, 47.71176265719419973, 6.012830585829961549 ) ) ;
#1806 =( BOUNDED_SURFACE ( )  B_SPLINE_SURFACE ( 3, 2, ( 
 ( #10816, #6765, #4460 ),
 ( #5527, #13516, #12198 ),
 ( #8888, #9025, #12339 ),
 ( #3424, #12272, #7862 ),
 ( #6845, #7637, #3358 ),
 ( #3495, #3279, #13386 ) ),
 .UNSPECIFIED., .F., .F., .T. ) 
 B_SPLINE_SURFACE_WITH_KNOTS ( ( 4, 2, 4 ),
 ( 3, 3 ),
 ( 0.01651999345535504898, 0.01858032176739834312, 0.02064065007944163380 ),
 ( 0.000000000000000000, 1.000000000000000000 ),
 .UNSPECIFIED. ) 
 GEOMETRIC_REPRESENTATION_ITEM ( )  RATIONAL_B_SPLINE_SURFACE ( (
 ( 1.000000000000000000, 0.8047781103519393575, 1.000000000000000000),
 ( 1.000000000000000000, 0.8123785825598874855, 1.000000000000000000),
 ( 1.000000000000000000, 0.8190671539795569833, 1.000000000000000000),
 ( 1.000000000000000000, 0.8192352254827578451, 1.000000000000000000),
 ( 1.000000000000000000, 0.8126129677217079905, 1.000000000000000000),
 ( 1.000000000000000000, 0.8047712537969728963, 1.000000000000000000) ) ) 
 REPRESENTATION_ITEM ( '' )  SURFACE ( )  );
#1807 = EDGE_LOOP ( 'NONE', ( #11288, #9763, #3211, #9884 ) ) ;
#1808 = CARTESIAN_POINT ( 'NONE',  ( 13.00000000000000533, 29.99999999999999289, 0.000000000000000000 ) ) ;
#1809 = ADVANCED_FACE ( 'NONE', ( #6293 ), #5056, .F. ) ;
#1810 = DIRECTION ( 'NONE',  ( 0.000000000000000000, 0.000000000000000000, 1.000000000000000000 ) ) ;
#1811 = CARTESIAN_POINT ( 'NONE',  ( 20.00000000000000711, 20.00000000000000355, 25.00000000000000000 ) ) ;
#1812 = CARTESIAN_POINT ( 'NONE',  ( 129.3408537872138595, 189.5765550933606107, -13.99999999999999645 ) ) ;
#1813 = AXIS2_PLACEMENT_3D ( 'NONE', #8430, #7399, #9537 ) ;
#1814 = ORIENTED_EDGE ( 'NONE', *, *, #7517, .T. ) ;
#1815 = LINE ( 'NONE', #6338, #5328 ) ;
#1816 = EDGE_CURVE ( 'NONE', #2047, #8757, #2506, .T. ) ;
#1817 = CARTESIAN_POINT ( 'NONE',  ( 1.654252653721915101, 3.663718938583012008, -0.01223254789873715748 ) ) ;
#1818 = VECTOR ( 'NONE', #11234, 1000.000000000000000 ) ;
#1819 = EDGE_CURVE ( 'NONE', #4025, #7502, #11428, .T. ) ;
#1820 = ORIENTED_EDGE ( 'NONE', *, *, #1404, .T. ) ;
#1821 = FACE_OUTER_BOUND ( 'NONE', #411, .T. ) ;
#1822 = ORIENTED_EDGE ( 'NONE', *, *, #6939, .F. ) ;
#1823 = ORIENTED_EDGE ( 'NONE', *, *, #7239, .F. ) ;
#1824 = FACE_OUTER_BOUND ( 'NONE', #8561, .T. ) ;
#1825 = ADVANCED_FACE ( 'NONE', ( #531 ), #9525, .T. ) ;
#1826 = LINE ( 'NONE', #1598, #6288 ) ;
#1827 = B_SPLINE_CURVE_WITH_KNOTS ( 'NONE', 3,
 ( #12263, #8814, #41, #8955, #3271, #5521 ),
 .UNSPECIFIED., .F., .F.,
 ( 4, 2, 4 ),
 ( 0.002365888236227998986, 0.003551327329835089319, 0.004736766423442179651 ),
 .UNSPECIFIED. ) ;
#1828 = FACE_OUTER_BOUND ( 'NONE', #10687, .T. ) ;
#1829 = DIRECTION ( 'NONE',  ( -1.000000000000000000, 1.892425610156516875E-16, 0.000000000000000000 ) ) ;
#1830 = AXIS2_PLACEMENT_3D ( 'NONE', #2192, #4329, #1009 ) ;
#1831 = DIRECTION ( 'NONE',  ( 0.000000000000000000, 1.000000000000000000, 0.000000000000000000 ) ) ;
#1832 = DIRECTION ( 'NONE',  ( -1.000000000000000000, -3.286707217423839940E-17, -2.273843122241288053E-18 ) ) ;
#1833 = CYLINDRICAL_SURFACE ( 'NONE', #4021, 4.599999999999999645 ) ;
#1834 = VECTOR ( 'NONE', #2821, 1000.000000000000227 ) ;
#1835 = CARTESIAN_POINT ( 'NONE',  ( 5.733169058567799681, -9.797989565831383431E-15, -6.438111078829122036 ) ) ;
#1836 = ORIENTED_EDGE ( 'NONE', *, *, #2559, .F. ) ;
#1837 = VECTOR ( 'NONE', #8930, 1000.000000000000000 ) ;
#1838 = EDGE_CURVE ( 'NONE', #9244, #1753, #14425, .T. ) ;
#1839 = VECTOR ( 'NONE', #13298, 1000.000000000000000 ) ;
#1840 = VERTEX_POINT ( 'NONE', #14283 ) ;
#1841 = ORIENTED_EDGE ( 'NONE', *, *, #1611, .T. ) ;
#1842 = CARTESIAN_POINT ( 'NONE',  ( 62.10586122665984732, -20.42344490663941414, -35.00000000000000000 ) ) ;
#1843 = CARTESIAN_POINT ( 'NONE',  ( 28.00000000000000355, 29.99999999999999645, -34.50000000000000000 ) ) ;
#1844 = EDGE_CURVE ( 'NONE', #6870, #2629, #3742, .T. ) ;
#1845 = AXIS2_PLACEMENT_3D ( 'NONE', #9928, #1142, #13382 ) ;
#1846 = EDGE_LOOP ( 'NONE', ( #9526, #2877, #13120, #11097 ) ) ;
#1847 = ORIENTED_EDGE ( 'NONE', *, *, #12373, .T. ) ;
#1848 = CARTESIAN_POINT ( 'NONE',  ( -0.1702248550645402425, -5.871782057790573717, -4.589066185948686538 ) ) ;
#1849 = DIRECTION ( 'NONE',  ( 1.000000000000000000, 0.000000000000000000, 0.000000000000000000 ) ) ;
#1850 = ORIENTED_EDGE ( 'NONE', *, *, #9598, .F. ) ;
#1851 = EDGE_CURVE ( 'NONE', #8043, #3245, #6575, .T. ) ;
#1852 = CARTESIAN_POINT ( 'NONE',  ( 57.35294117647057277, -1.411764705882362358, -25.00000000000000000 ) ) ;
#1853 = ORIENTED_EDGE ( 'NONE', *, *, #13064, .T. ) ;
#1854 = LINE ( 'NONE', #10984, #945 ) ;
#1855 = LINE ( 'NONE', #7254, #8774 ) ;
#1856 = CARTESIAN_POINT ( 'NONE',  ( 1.057097118173367415E-15, -0.3908539631446322216, 4.000000000000004441 ) ) ;
#1857 = VERTEX_POINT ( 'NONE', #13124 ) ;
#1858 = FACE_OUTER_BOUND ( 'NONE', #1072, .T. ) ;
#1859 = FACE_OUTER_BOUND ( 'NONE', #4265, .T. ) ;
#1860 = FILL_AREA_STYLE_COLOUR ( '', #12668 ) ;
#1861 = VERTEX_POINT ( 'NONE', #4274 ) ;
#1862 = PLANE ( 'NONE',  #12207 ) ;
#1863 = ORIENTED_EDGE ( 'NONE', *, *, #8702, .F. ) ;
#1864 = CARTESIAN_POINT ( 'NONE',  ( 36.31750732272606541, 144.5765550933605823, -199.4258611313499330 ) ) ;
#1865 = VERTEX_POINT ( 'NONE', #8711 ) ;
#1866 = CARTESIAN_POINT ( 'NONE',  ( 3.903127820947815962E-15, 5.773502691896270633, -0.5999999999999894307 ) ) ;
#1867 = CARTESIAN_POINT ( 'NONE',  ( -0.02448804030508153901, -4.877043185438141748, -3.451162025751979279 ) ) ;
#1868 = AXIS2_PLACEMENT_3D ( 'NONE', #9436, #2790, #7226 ) ;
#1869 = ORIENTED_EDGE ( 'NONE', *, *, #9807, .F. ) ;
#1870 = FACE_OUTER_BOUND ( 'NONE', #486, .T. ) ;
#1871 = ADVANCED_FACE ( 'NONE', ( #12299 ), #3099, .F. ) ;
#1872 = CYLINDRICAL_SURFACE ( 'NONE', #9645, 4.750000000000000000 ) ;
#1873 = EDGE_CURVE ( 'NONE', #269, #11894, #10364, .T. ) ;
#1874 = EDGE_LOOP ( 'NONE', ( #2929, #7336, #11493, #6111 ) ) ;
#1875 = ORIENTED_EDGE ( 'NONE', *, *, #12362, .T. ) ;
#1876 = DIRECTION ( 'NONE',  ( 1.000000000000000000, 0.000000000000000000, 0.000000000000000000 ) ) ;
#1877 = CARTESIAN_POINT ( 'NONE',  ( 28.00000000000000355, 29.99999999999999645, 25.00000000000000000 ) ) ;
#1878 = ORIENTED_EDGE ( 'NONE', *, *, #12626, .F. ) ;
#1879 = CARTESIAN_POINT ( 'NONE',  ( 5.091953023115930677, -2.341213539480237582, 4.055100801747969719 ) ) ;
#1880 = VECTOR ( 'NONE', #857, 1000.000000000000114 ) ;
#1881 = DIRECTION ( 'NONE',  ( 0.9701425001453319874, 0.2425356250363328026, 0.000000000000000000 ) ) ;
#1882 = CARTESIAN_POINT ( 'NONE',  ( 20.00000000000000000, -5.510910596163090344E-15, -25.00000000000000000 ) ) ;
#1883 = PLANE ( 'NONE',  #3706 ) ;
#1884 = ORIENTED_EDGE ( 'NONE', *, *, #13910, .F. ) ;
#1885 =( NAMED_UNIT ( * ) PLANE_ANGLE_UNIT ( ) SI_UNIT ( $, .RADIAN. ) );
#1886 = CARTESIAN_POINT ( 'NONE',  ( 57.35294117647057277, -1.411764705882362358, 23.00000000000000000 ) ) ;
#1887 = CARTESIAN_POINT ( 'NONE',  ( 20.00000000000000000, 27.00000000000000355, 25.00000000000000000 ) ) ;
#1888 = AXIS2_PLACEMENT_3D ( 'NONE', #7294, #2996, #12863 ) ;
#1889 = EDGE_CURVE ( 'NONE', #1368, #8027, #8777, .T. ) ;
#1890 = AXIS2_PLACEMENT_3D ( 'NONE', #7851, #2239, #984 ) ;
#1891 = ORIENTED_EDGE ( 'NONE', *, *, #3210, .F. ) ;
#1892 = ORIENTED_EDGE ( 'NONE', *, *, #12248, .T. ) ;
#1893 = DIRECTION ( 'NONE',  ( 0.000000000000000000, 0.000000000000000000, -1.000000000000000000 ) ) ;
#1894 = ORIENTED_EDGE ( 'NONE', *, *, #6821, .F. ) ;
#1895 = ORIENTED_EDGE ( 'NONE', *, *, #1579, .F. ) ;
#1896 = CARTESIAN_POINT ( 'NONE',  ( 22.00000000000000000, 57.00000000000000000, -25.00000000000000000 ) ) ;
#1897 = CARTESIAN_POINT ( 'NONE',  ( 31.38313257588138683, 143.6985259526510390, -28.00000000000000000 ) ) ;
#1898 = DIRECTION ( 'NONE',  ( -1.000000000000000000, 0.000000000000000000, 0.000000000000000000 ) ) ;
#1899 = VECTOR ( 'NONE', #1028, 1000.000000000000114 ) ;
#1900 = FACE_OUTER_BOUND ( 'NONE', #3304, .T. ) ;
#1901 = CARTESIAN_POINT ( 'NONE',  ( 25.90000000000000213, 29.99999999999999645, 6.999999999999992006 ) ) ;
#1902 = APPLICATION_PROTOCOL_DEFINITION ( 'draft international standard', 'automotive_design', 1998, #7358 ) ;
#1903 = FACE_OUTER_BOUND ( 'NONE', #10336, .T. ) ;
#1904 = MANIFOLD_SOLID_BREP ( 'Boss-Extrude1', #11798 ) ;
#1905 = CIRCLE ( 'NONE', #9829, 0.4999999999999978351 ) ;
#1906 = DIRECTION ( 'NONE',  ( 1.000000000000000000, 0.000000000000000000, 0.000000000000000000 ) ) ;
#1907 = ORIENTED_EDGE ( 'NONE', *, *, #5733, .T. ) ;
#1908 = LINE ( 'NONE', #3092, #14326 ) ;
#1909 = ADVANCED_FACE ( 'NONE', ( #5485 ), #13413, .F. ) ;
#1910 = ORIENTED_EDGE ( 'NONE', *, *, #12743, .F. ) ;
#1911 = ADVANCED_FACE ( 'NONE', ( #13331 ), #6651, .T. ) ;
#1912 = CIRCLE ( 'NONE', #11248, 8.000000000000000000 ) ;
#1913 = MECHANICAL_DESIGN_GEOMETRIC_PRESENTATION_REPRESENTATION (  '', ( #8198 ), #10307 ) ;
#1914 = CIRCLE ( 'NONE', #11959, 4.999999999999976907 ) ;
#1915 = CARTESIAN_POINT ( 'NONE',  ( 4.872112557124452792, -0.7838640816432008718, -4.072377784234222808 ) ) ;
#1916 = VERTEX_POINT ( 'NONE', #3385 ) ;
#1917 = DIRECTION ( 'NONE',  ( 0.000000000000000000, 0.000000000000000000, -1.000000000000000000 ) ) ;
#1918 = CARTESIAN_POINT ( 'NONE',  ( -1.295960409299079124E-15, 0.3423821193476913050, 3.499999999999996003 ) ) ;
#1919 = EDGE_CURVE ( 'NONE', #1840, #11047, #9738, .T. ) ;
#1920 = CIRCLE ( 'NONE', #8926, 9.000000000000005329 ) ;
#1921 = ADVANCED_FACE ( 'NONE', ( #11186 ), #12517, .F. ) ;
#1922 = ORIENTED_EDGE ( 'NONE', *, *, #4515, .T. ) ;
#1923 = AXIS2_PLACEMENT_3D ( 'NONE', #4562, #13481, #7898 ) ;
#1924 = AXIS2_PLACEMENT_3D ( 'NONE', #7914, #10455, #3739 ) ;
#1925 = FACE_OUTER_BOUND ( 'NONE', #13791, .T. ) ;
#1926 = CARTESIAN_POINT ( 'NONE',  ( 4.988724804725896966, 2.309401076758504701, 4.000000000000031086 ) ) ;
#1927 = FACE_OUTER_BOUND ( 'NONE', #1803, .T. ) ;
#1928 = AXIS2_PLACEMENT_3D ( 'NONE', #11960, #10917, #1936 ) ;
#1929 = ORIENTED_EDGE ( 'NONE', *, *, #7016, .T. ) ;
#1930 = VECTOR ( 'NONE', #5761, 1000.000000000000000 ) ;
#1931 = CARTESIAN_POINT ( 'NONE',  ( 59.18121602037099649, 13.58289998256015352, -25.00000000000000000 ) ) ;
#1932 = CARTESIAN_POINT ( 'NONE',  ( 54.25585977000769589, 23.28432498401347672, 25.00000000000000000 ) ) ;
#1933 = CARTESIAN_POINT ( 'NONE',  ( -68.68170757442787533, -83.66032599071911591, -106.9999999999999858 ) ) ;
#1934 = VERTEX_POINT ( 'NONE', #365 ) ;
#1935 = CARTESIAN_POINT ( 'NONE',  ( 21.68170757442808849, 141.2731697022877313, -28.00000000000000000 ) ) ;
#1936 = DIRECTION ( 'NONE',  ( -1.000000000000000000, 0.000000000000000000, 0.000000000000000000 ) ) ;
#1937 =( LENGTH_UNIT ( ) NAMED_UNIT ( * ) SI_UNIT ( .MILLI., .METRE. ) );
#1938 = EDGE_CURVE ( 'NONE', #950, #13670, #9058, .T. ) ;
#1939 = CARTESIAN_POINT ( 'NONE',  ( 2.540000000000002700, 4.229949723821848943E-16, 1.599999999999990319 ) ) ;
#1940 = ORIENTED_EDGE ( 'NONE', *, *, #8566, .F. ) ;
#1941 = CYLINDRICAL_SURFACE ( 'NONE', #12796, 5.000000000000004441 ) ;
#1942 =( GEOMETRIC_REPRESENTATION_CONTEXT ( 3 ) GLOBAL_UNCERTAINTY_ASSIGNED_CONTEXT ( ( #12748 ) ) GLOBAL_UNIT_ASSIGNED_CONTEXT ( ( #1791, #9544, #8437 ) ) REPRESENTATION_CONTEXT ( 'NONE', 'WORKASPACE' ) );
#1943 = CIRCLE ( 'NONE', #8007, 3.299999999999983391 ) ;
#1944 = CIRCLE ( 'NONE', #3354, 4.000000000000004441 ) ;
#1945 = FACE_OUTER_BOUND ( 'NONE', #3904, .T. ) ;
#1946 = ORIENTED_EDGE ( 'NONE', *, *, #6197, .F. ) ;
#1947 = DIRECTION ( 'NONE',  ( 1.000000000000000000, 1.665334536937734564E-16, 0.000000000000000000 ) ) ;
#1948 = CARTESIAN_POINT ( 'NONE',  ( 4.851472949721052252, -1.539600717838985666, 4.000000000000002665 ) ) ;
#1949 = ORIENTED_EDGE ( 'NONE', *, *, #5722, .F. ) ;
#1950 = ORIENTED_EDGE ( 'NONE', *, *, #53, .F. ) ;
#1951 = DIRECTION ( 'NONE',  ( 0.000000000000000000, 0.000000000000000000, -1.000000000000000000 ) ) ;
#1952 = DIRECTION ( 'NONE',  ( -1.000000000000000000, -3.286707217423839940E-17, -2.273843122241288053E-18 ) ) ;
#1953 = AXIS2_PLACEMENT_3D ( 'NONE', #7106, #11430, #5005 ) ;
#1954 = VERTEX_POINT ( 'NONE', #4820 ) ;
#1955 = CARTESIAN_POINT ( 'NONE',  ( -118.6817075744282306, 109.5765550933602697, -3.299999999999983391 ) ) ;
#1956 = VECTOR ( 'NONE', #1485, 1000.000000000000000 ) ;
#1957 = CARTESIAN_POINT ( 'NONE',  ( 0.000000000000000000, 4.618802153517023612, 0.000000000000000000 ) ) ;
#1958 = CARTESIAN_POINT ( 'NONE',  ( -24.99999999999998934, -30.42444490663959300, -2.000000000000001776 ) ) ;
#1959 = B_SPLINE_CURVE_WITH_KNOTS ( 'NONE', 3,
 ( #12836, #13066, #825, #11739, #2968, #13938, #2820, #3847, #10563, #4143, #7259, #6385, #10640, #1715, #9690, #11656 ),
 .UNSPECIFIED., .F., .F.,
 ( 4, 3, 3, 3, 3, 4 ),
 ( 0.000000000000000000, 3.315506744709155554E-05, 6.608280158698769959E-05, 0.0001026520855291340468, 0.0001376952025664801528, 0.0001398064759190615887 ),
 .UNSPECIFIED. ) ;
#1960 = ADVANCED_FACE ( 'NONE', ( #5821 ), #6764, .T. ) ;
#1961 = CARTESIAN_POINT ( 'NONE',  ( 1.560000000000005826, -0.8660254037844428154, -1.500000000000001332 ) ) ;
#1962 = EDGE_CURVE ( 'NONE', #13737, #768, #215, .T. ) ;
#1963 = DIRECTION ( 'NONE',  ( 0.000000000000000000, -0.000000000000000000, -1.000000000000000000 ) ) ;
#1964 = AXIS2_PLACEMENT_3D ( 'NONE', #13099, #5530, #8824 ) ;
#1965 = DIRECTION ( 'NONE',  ( -1.000000000000000000, -3.286707217423839940E-17, -2.273843122241288053E-18 ) ) ;
#1966 = CARTESIAN_POINT ( 'NONE',  ( 2.000000000000015543, 3.464101615137753942, 0.000000000000000000 ) ) ;
#1967 = AXIS2_PLACEMENT_3D ( 'NONE', #4821, #13841, #8319 ) ;
#1968 = ORIENTED_EDGE ( 'NONE', *, *, #1057, .F. ) ;
#1969 = ORIENTED_EDGE ( 'NONE', *, *, #4883, .F. ) ;
#1970 = EDGE_LOOP ( 'NONE', ( #11011, #9719, #183, #4660, #1968 ) ) ;
#1971 = DIRECTION ( 'NONE',  ( 1.000000000000000000, 1.927470528863119049E-16, 0.000000000000000000 ) ) ;
#1972 = ORIENTED_EDGE ( 'NONE', *, *, #2543, .T. ) ;
#1973 = PLANE ( 'NONE',  #10047 ) ;
#1974 = CARTESIAN_POINT ( 'NONE',  ( 20.00000000000000000, -5.510910596163090344E-15, -25.00000000000000000 ) ) ;
#1975 = CARTESIAN_POINT ( 'NONE',  ( 20.00000000000000000, 78.00000000000000000, -25.00000000000000000 ) ) ;
#1976 = LINE ( 'NONE', #4258, #14222 ) ;
#1977 = FACE_OUTER_BOUND ( 'NONE', #8291, .T. ) ;
#1978 = PRODUCT_CONTEXT ( 'NONE', #7358, 'mechanical' ) ;
#1979 = FACE_OUTER_BOUND ( 'NONE', #5149, .T. ) ;
#1980 = DIRECTION ( 'NONE',  ( 0.000000000000000000, 0.000000000000000000, -1.000000000000000000 ) ) ;
#1981 = ORIENTED_EDGE ( 'NONE', *, *, #7232, .F. ) ;
#1982 =( BOUNDED_SURFACE ( )  B_SPLINE_SURFACE ( 3, 2, ( 
 ( #6467, #10941, #5380 ),
 ( #990, #9849, #14325 ),
 ( #5454, #14395, #11154 ),
 ( #6965, #8884, #5656 ),
 ( #12475, #12534, #4524 ),
 ( #10195, #5718, #8063 ) ),
 .UNSPECIFIED., .F., .F., .T. ) 
 B_SPLINE_SURFACE_WITH_KNOTS ( ( 4, 2, 4 ),
 ( 3, 3 ),
 ( 0.002450104044831662078, 0.005591829551853649133, 0.008733555058875635754 ),
 ( 0.000000000000000000, 1.000000000000000000 ),
 .UNSPECIFIED. ) 
 GEOMETRIC_REPRESENTATION_ITEM ( )  RATIONAL_B_SPLINE_SURFACE ( (
 ( 1.000000000000000000, 0.8047731410850403888, 1.000000000000000000),
 ( 1.000000000000000000, 0.8125552299157110525, 1.000000000000000000),
 ( 1.000000000000000000, 0.8191520442888688969, 1.000000000000000000),
 ( 1.000000000000000000, 0.8191520442891042642, 1.000000000000000000),
 ( 1.000000000000000000, 0.8125552299155337499, 1.000000000000000000),
 ( 1.000000000000000000, 0.8047731410850403888, 1.000000000000000000) ) ) 
 REPRESENTATION_ITEM ( '' )  SURFACE ( )  );
#1983 = EDGE_CURVE ( 'NONE', #12581, #2621, #1241, .T. ) ;
#1984 = CARTESIAN_POINT ( 'NONE',  ( 4.170895651974822371, -2.054890354522667995, 3.559174498016340227 ) ) ;
#1985 = VERTEX_POINT ( 'NONE', #296 ) ;
#1986 = ORIENTED_EDGE ( 'NONE', *, *, #37, .F. ) ;
#1987 = CARTESIAN_POINT ( 'NONE',  ( 79.68170757442804586, 59.57655509336061073, 25.00000000000000000 ) ) ;
#1988 = DIRECTION ( 'NONE',  ( -1.000000000000000000, 0.000000000000000000, 0.000000000000000000 ) ) ;
#1989 = CARTESIAN_POINT ( 'NONE',  ( 0.3126073911696169993, 2.020725942163681399, -3.499999999999996003 ) ) ;
#1990 = CIRCLE ( 'NONE', #7575, 3.299999999999969624 ) ;
#1991 = CARTESIAN_POINT ( 'NONE',  ( 44.62907851819101523, 71.79144999128007498, 25.00000000000000000 ) ) ;
#1992 = EDGE_CURVE ( 'NONE', #8895, #4249, #13765, .T. ) ;
#1993 = ORIENTED_EDGE ( 'NONE', *, *, #13450, .F. ) ;
#1994 = B_SPLINE_CURVE_WITH_KNOTS ( 'NONE', 3,
 ( #9739, #2209, #11188, #8712, #10971, #8779 ),
 .UNSPECIFIED., .F., .F.,
 ( 4, 2, 4 ),
 ( 0.002336974151641544283, 0.003500975885716459297, 0.004664977619791374312 ),
 .UNSPECIFIED. ) ;
#1995 = DIRECTION ( 'NONE',  ( 1.000000000000000000, 0.000000000000000000, -3.576224061345501491E-16 ) ) ;
#1996 = LINE ( 'NONE', #12988, #749 ) ;
#1997 = MANIFOLD_SOLID_BREP ( 'FlangeHexFillet', #343 ) ;
#1998 = CARTESIAN_POINT ( 'NONE',  ( 0.000000000000000000, 48.49999999999999289, 0.000000000000000000 ) ) ;
#1999 = EDGE_CURVE ( 'NONE', #11064, #10506, #2413, .T. ) ;
#2000 = CARTESIAN_POINT ( 'NONE',  ( 20.00000000000000000, -5.510910596163090344E-15, -25.00000000000000000 ) ) ;
#2001 = FACE_OUTER_BOUND ( 'NONE', #12684, .T. ) ;
#2002 = DIRECTION ( 'NONE',  ( -0.000000000000000000, -0.000000000000000000, -1.000000000000000000 ) ) ;
#2003 = DIRECTION ( 'NONE',  ( 0.000000000000000000, 4.440892098500620738E-16, 1.000000000000000000 ) ) ;
#2004 = PLANE ( 'NONE',  #4907 ) ;
#2005 = EDGE_CURVE ( 'NONE', #9291, #5102, #9129, .T. ) ;
#2006 = CARTESIAN_POINT ( 'NONE',  ( 20.00000000000000711, 20.00000000000000355, -25.00000000000000000 ) ) ;
#2007 = EDGE_LOOP ( 'NONE', ( #10274, #2455, #12573, #207 ) ) ;
#2008 = ORIENTED_EDGE ( 'NONE', *, *, #2079, .T. ) ;
#2009 = ORIENTED_EDGE ( 'NONE', *, *, #936, .T. ) ;
#2010 = DIRECTION ( 'NONE',  ( -0.5000000000000014433, -0.8660254037844378194, 0.000000000000000000 ) ) ;
#2011 = DIRECTION ( 'NONE',  ( 0.000000000000000000, 0.000000000000000000, -1.000000000000000000 ) ) ;
#2012 = ORIENTED_EDGE ( 'NONE', *, *, #12789, .F. ) ;
#2013 = DIRECTION ( 'NONE',  ( 0.8191520442889900222, 2.367334119411125886E-16, -0.5735764363510484909 ) ) ;
#2014 = CARTESIAN_POINT ( 'NONE',  ( 5.253368672218637236, -3.033033817057797510, -4.659491423763650886 ) ) ;
#2015 = ORIENTED_EDGE ( 'NONE', *, *, #9070, .F. ) ;
#2016 = EDGE_CURVE ( 'NONE', #1217, #11907, #9581, .T. ) ;
#2017 = ORIENTED_EDGE ( 'NONE', *, *, #11143, .T. ) ;
#2018 = DIRECTION ( 'NONE',  ( -1.000000000000000000, 0.000000000000000000, 0.000000000000000000 ) ) ;
#2019 = DIRECTION ( 'NONE',  ( 1.000000000000000000, 0.000000000000000000, 0.000000000000000000 ) ) ;
#2020 = ORIENTED_EDGE ( 'NONE', *, *, #6153, .F. ) ;
#2021 = CARTESIAN_POINT ( 'NONE',  ( 3.878096787214416530, -3.381939201670113526, -1.142309474598453667 ) ) ;
#2022 = DIRECTION ( 'NONE',  ( -1.000000000000000000, 2.551526159633733968E-19, 1.987661601597216239E-18 ) ) ;
#2023 = CARTESIAN_POINT ( 'NONE',  ( -2.500000000000000444, 3.775608651740452848E-15, -0.3501037691048258793 ) ) ;
#2024 = CYLINDRICAL_SURFACE ( 'NONE', #7905, 2.500000000000002220 ) ;
#2025 = CARTESIAN_POINT ( 'NONE',  ( -140.0000000000003411, 189.5765550933606107, -132.0000000000000000 ) ) ;
#2026 = CARTESIAN_POINT ( 'NONE',  ( 5.103531824934171013, 4.708196996972911386, -1.387778780781445676E-14 ) ) ;
#2027 = VECTOR ( 'NONE', #13139, 1000.000000000000000 ) ;
#2028 = ORIENTED_EDGE ( 'NONE', *, *, #1154, .T. ) ;
#2029 = ADVANCED_FACE ( 'NONE', ( #13912 ), #9800, .T. ) ;
#2030 = EDGE_CURVE ( 'NONE', #619, #2684, #5361, .T. ) ;
#2031 = ORIENTED_EDGE ( 'NONE', *, *, #4339, .T. ) ;
#2032 = CARTESIAN_POINT ( 'NONE',  ( -2.134523027080836066E-15, -0.3420925509381486651, -3.499999999999995115 ) ) ;
#2033 = VERTEX_POINT ( 'NONE', #9434 ) ;
#2034 = DIRECTION ( 'NONE',  ( 0.000000000000000000, 0.000000000000000000, -1.000000000000000000 ) ) ;
#2035 = PLANE ( 'NONE',  #4449 ) ;
#2036 = CARTESIAN_POINT ( 'NONE',  ( 118.6817075744280316, 69.57655509336046862, 3.299999999999982947 ) ) ;
#2037 = PLANE ( 'NONE',  #6947 ) ;
#2038 = AXIS2_PLACEMENT_3D ( 'NONE', #3992, #397, #8135 ) ;
#2039 = LINE ( 'NONE', #7733, #7005 ) ;
#2040 = SHAPE_DEFINITION_REPRESENTATION ( #4978, #4344 ) ;
#2041 = DIRECTION ( 'NONE',  ( 0.9701425001453325425, 0.2425356250363304988, 0.000000000000000000 ) ) ;
#2042 = CYLINDRICAL_SURFACE ( 'NONE', #4497, 5.499999999999984013 ) ;
#2043 = CIRCLE ( 'NONE', #7627, 3.299999999999997158 ) ;
#2044 = AXIS2_PLACEMENT_3D ( 'NONE', #5674, #133, #6854 ) ;
#2045 = ORIENTED_EDGE ( 'NONE', *, *, #5645, .T. ) ;
#2046 = CARTESIAN_POINT ( 'NONE',  ( 46.97979101891770171, 52.38859998837343568, 25.00000000000000000 ) ) ;
#2047 = VERTEX_POINT ( 'NONE', #5109 ) ;
#2048 = CARTESIAN_POINT ( 'NONE',  ( -5.000000000000000000, 2.886751345948124214, -4.284345921091780696 ) ) ;
#2049 = VECTOR ( 'NONE', #4297, 1000.000000000000000 ) ;
#2050 = ORIENTED_EDGE ( 'NONE', *, *, #4383, .F. ) ;
#2051 = CIRCLE ( 'NONE', #8821, 4.999999999999988454 ) ;
#2052 = CARTESIAN_POINT ( 'NONE',  ( 71.80728622811317052, -20.42344490663941414, -27.99999999999999645 ) ) ;
#2053 = DIRECTION ( 'NONE',  ( 0.000000000000000000, 0.000000000000000000, -1.000000000000000000 ) ) ;
#2054 = DIRECTION ( 'NONE',  ( -1.000000000000000000, 0.000000000000000000, 0.000000000000000000 ) ) ;
#2055 = EDGE_CURVE ( 'NONE', #5455, #14165, #5973, .T. ) ;
#2056 = CARTESIAN_POINT ( 'NONE',  ( 4.873329151231342138, 3.940175375302556127, -1.320232820537355245 ) ) ;
#2057 = ORIENTED_EDGE ( 'NONE', *, *, #10089, .T. ) ;
#2058 = AXIS2_PLACEMENT_3D ( 'NONE', #13499, #3616, #3752 ) ;
#2059 = DIRECTION ( 'NONE',  ( -1.000000000000000000, -1.665334536937734071E-16, 0.000000000000000000 ) ) ;
#2060 = VECTOR ( 'NONE', #6406, 1000.000000000000114 ) ;
#2061 = DIRECTION ( 'NONE',  ( -1.000000000000000000, 0.000000000000000000, 0.000000000000000000 ) ) ;
#2062 = VECTOR ( 'NONE', #11153, 1000.000000000000000 ) ;
#2063 = DIRECTION ( 'NONE',  ( -0.2425356250363328581, 0.9701425001453318764, 0.000000000000000000 ) ) ;
#2064 = EDGE_CURVE ( 'NONE', #3193, #1507, #9654, .T. ) ;
#2065 = EDGE_CURVE ( 'NONE', #2858, #254, #4035, .T. ) ;
#2066 = FACE_OUTER_BOUND ( 'NONE', #4145, .T. ) ;
#2067 = DIRECTION ( 'NONE',  ( -1.000000000000000000, 0.000000000000000000, 0.000000000000000000 ) ) ;
#2068 = DIRECTION ( 'NONE',  ( 0.000000000000000000, 1.000000000000000000, -0.000000000000000000 ) ) ;
#2069 = LINE ( 'NONE', #1187, #2027 ) ;
#2070 = EDGE_CURVE ( 'NONE', #9480, #12696, #4893, .T. ) ;
#2071 = VECTOR ( 'NONE', #122, 1000.000000000000000 ) ;
#2072 = CARTESIAN_POINT ( 'NONE',  ( 36.99999999999999289, 80.00000000000000000, -25.00000000000000000 ) ) ;
#2073 = DIRECTION ( 'NONE',  ( 0.000000000000000000, -0.000000000000000000, -1.000000000000000000 ) ) ;
#2074 = PRESENTATION_STYLE_ASSIGNMENT (( #13069 ) ) ;
#2075 = CIRCLE ( 'NONE', #10242, 2.055000000000000160 ) ;
#2076 = DIRECTION ( 'NONE',  ( 0.000000000000000000, 0.000000000000000000, -1.000000000000000000 ) ) ;
#2077 = ORIENTED_EDGE ( 'NONE', *, *, #5682, .F. ) ;
#2078 = LINE ( 'NONE', #3409, #8110 ) ;
#2079 = EDGE_CURVE ( 'NONE', #3573, #12564, #513, .T. ) ;
#2080 = ORIENTED_EDGE ( 'NONE', *, *, #12073, .T. ) ;
#2081 = DIRECTION ( 'NONE',  ( -0.000000000000000000, -0.000000000000000000, 1.000000000000000000 ) ) ;
#2082 = DIRECTION ( 'NONE',  ( 1.000000000000000000, 8.619211990076297369E-16, 0.000000000000000000 ) ) ;
#2083 = CIRCLE ( 'NONE', #6471, 0.5155456020628804703 ) ;
#2084 = EDGE_CURVE ( 'NONE', #10580, #1563, #11781, .T. ) ;
#2085 = EDGE_CURVE ( 'NONE', #6341, #10817, #1826, .T. ) ;
#2086 = VERTEX_POINT ( 'NONE', #13840 ) ;
#2087 = ORIENTED_EDGE ( 'NONE', *, *, #3724, .T. ) ;
#2088 = FACE_OUTER_BOUND ( 'NONE', #13599, .T. ) ;
#2089 = LINE ( 'NONE', #6752, #7978 ) ;
#2090 = EDGE_CURVE ( 'NONE', #9523, #5064, #594, .T. ) ;
#2091 = CARTESIAN_POINT ( 'NONE',  ( 4.033901012036043454, -2.321269032826913659, -2.979444097106994427 ) ) ;
#2092 = DIRECTION ( 'NONE',  ( -1.723842398015259277E-15, 1.000000000000000000, 0.000000000000000000 ) ) ;
#2093 = DIRECTION ( 'NONE',  ( 0.000000000000000000, 0.000000000000000000, -1.000000000000000000 ) ) ;
#2094 = CARTESIAN_POINT ( 'NONE',  ( 4.086376210449946811, 2.103254844323302564, 3.499999999999992450 ) ) ;
#2095 = ORIENTED_EDGE ( 'NONE', *, *, #2070, .F. ) ;
#2096 = CARTESIAN_POINT ( 'NONE',  ( -118.6817075744279748, -20.42344490663959178, 33.00000000000002842 ) ) ;
#2097 = AXIS2_PLACEMENT_3D ( 'NONE', #65, #12421, #13311 ) ;
#2098 = DIRECTION ( 'NONE',  ( 0.000000000000000000, 0.000000000000000000, -1.000000000000000000 ) ) ;
#2099 = ADVANCED_FACE ( 'NONE', ( #10750 ), #10503, .T. ) ;
#2100 = VECTOR ( 'NONE', #2190, 1000.000000000000000 ) ;
#2101 = DIRECTION ( 'NONE',  ( 0.000000000000000000, 0.000000000000000000, -1.000000000000000000 ) ) ;
#2102 = ORIENTED_EDGE ( 'NONE', *, *, #13571, .F. ) ;
#2103 = ORIENTED_EDGE ( 'NONE', *, *, #3418, .F. ) ;
#2104 = ORIENTED_EDGE ( 'NONE', *, *, #7153, .F. ) ;
#2105 = AXIS2_PLACEMENT_3D ( 'NONE', #3365, #132, #1077 ) ;
#2106 = CARTESIAN_POINT ( 'NONE',  ( 0.000000000000000000, 40.49999999999999289, 8.000000000000007105 ) ) ;
#2107 = VERTEX_POINT ( 'NONE', #9509 ) ;
#2108 = DIRECTION ( 'NONE',  ( 0.000000000000000000, 0.000000000000000000, -1.000000000000000000 ) ) ;
#2109 = FACE_OUTER_BOUND ( 'NONE', #10942, .T. ) ;
#2110 = CARTESIAN_POINT ( 'NONE',  ( 61.68121602037100359, 13.58289998256015352, -25.00000000000000000 ) ) ;
#2111 = DIRECTION ( 'NONE',  ( 0.000000000000000000, -1.000000000000000000, 0.000000000000000000 ) ) ;
#2112 = DIRECTION ( 'NONE',  ( 0.000000000000000000, 0.000000000000000000, -1.000000000000000000 ) ) ;
#2113 = CONTEXT_DEPENDENT_SHAPE_REPRESENTATION ( #4023, #8598 ) ;
#2114 = DIRECTION ( 'NONE',  ( 0.000000000000000000, 0.000000000000000000, -1.000000000000000000 ) ) ;
#2115 = EDGE_CURVE ( 'NONE', #2459, #5279, #11552, .T. ) ;
#2116 = CARTESIAN_POINT ( 'NONE',  ( 4.151274195509661702, 2.039912954708745563, -3.533232880573503376 ) ) ;
#2117 = CIRCLE ( 'NONE', #12161, 2.500000000000002220 ) ;
#2118 = AXIS2_PLACEMENT_3D ( 'NONE', #5069, #7337, #3911 ) ;
#2119 = ORIENTED_EDGE ( 'NONE', *, *, #1730, .F. ) ;
#2120 = CARTESIAN_POINT ( 'NONE',  ( 4.988724804725896966, 2.309401076758504701, 4.000000000000031086 ) ) ;
#2121 = ORIENTED_EDGE ( 'NONE', *, *, #11840, .F. ) ;
#2122 = ORIENTED_EDGE ( 'NONE', *, *, #327, .F. ) ;
#2123 = LINE ( 'NONE', #12076, #5253 ) ;
#2124 = VECTOR ( 'NONE', #8164, 1000.000000000000000 ) ;
#2125 = ORIENTED_EDGE ( 'NONE', *, *, #11328, .F. ) ;
#2126 = DIRECTION ( 'NONE',  ( 0.000000000000000000, 0.000000000000000000, 1.000000000000000000 ) ) ;
#2127 = CONICAL_SURFACE ( 'NONE', #3306, 3.499999999999999112, 1.047197551196600296 ) ;
#2128 = CARTESIAN_POINT ( 'NONE',  ( 57.35294117647057277, -1.411764705882362358, 25.00000000000000000 ) ) ;
#2129 = CARTESIAN_POINT ( 'NONE',  ( 30.10000000000000497, 29.99999999999999645, 25.00000000000000000 ) ) ;
#2130 = CARTESIAN_POINT ( 'NONE',  ( 30.60000000000000853, 29.99999999999999645, -24.99999999999999289 ) ) ;
#2131 = ORIENTED_EDGE ( 'NONE', *, *, #3606, .F. ) ;
#2132 = LINE ( 'NONE', #6724, #14200 ) ;
#2133 = CARTESIAN_POINT ( 'NONE',  ( 3.333333333333336146, -2.694301256218264662, -3.000726591567077328 ) ) ;
#2134 = SURFACE_STYLE_FILL_AREA ( #10975 ) ;
#2135 = CIRCLE ( 'NONE', #1660, 2.540000000000002700 ) ;
#2136 = EDGE_CURVE ( 'NONE', #8708, #663, #6209, .T. ) ;
#2137 = DIRECTION ( 'NONE',  ( 1.000000000000000000, 1.665334536937734318E-16, 0.000000000000000000 ) ) ;
#2138 = ORIENTED_EDGE ( 'NONE', *, *, #2659, .F. ) ;
#2139 = EDGE_CURVE ( 'NONE', #5220, #1840, #12145, .T. ) ;
#2140 = CARTESIAN_POINT ( 'NONE',  ( 8.000000000000000000, 25.49999999999996803, 0.000000000000000000 ) ) ;
#2141 = AXIS2_PLACEMENT_3D ( 'NONE', #7308, #12969, #3815 ) ;
#2142 = CARTESIAN_POINT ( 'NONE',  ( 22.00000000000000000, 70.00000000000000000, -25.00000000000000000 ) ) ;
#2143 = DIRECTION ( 'NONE',  ( 0.9701425001453319874, 0.2425356250363330801, 0.000000000000000000 ) ) ;
#2144 = CIRCLE ( 'NONE', #4024, 9.000000000000001776 ) ;
#2145 = ORIENTED_EDGE ( 'NONE', *, *, #10928, .F. ) ;
#2146 = CARTESIAN_POINT ( 'NONE',  ( 51.90514726928103073, 42.68717498692012668, 25.00000000000000000 ) ) ;
#2147 = CARTESIAN_POINT ( 'NONE',  ( 1.560000000000005826, 0.8660254037844428154, -1.500000000000001332 ) ) ;
#2148 = FACE_OUTER_BOUND ( 'NONE', #13063, .T. ) ;
#2149 = DIRECTION ( 'NONE',  ( 0.000000000000000000, 0.000000000000000000, 1.000000000000000000 ) ) ;
#2150 = B_SPLINE_CURVE_WITH_KNOTS ( 'NONE', 3,
 ( #7764, #12238, #7601, #12085 ),
 .UNSPECIFIED., .F., .F.,
 ( 4, 4 ),
 ( 2.380739282789443030E-07, 0.002044882221487529742 ),
 .UNSPECIFIED. ) ;
#2151 = CIRCLE ( 'NONE', #10317, 2.500000000000002220 ) ;
#2152 = DIRECTION ( 'NONE',  ( 0.000000000000000000, 0.000000000000000000, -1.000000000000000000 ) ) ;
#2153 = COLOUR_RGB ( '', 0.66274510, 0.83137255, 0.94901961) ;
#2154 = VECTOR ( 'NONE', #12374, 1000.000000000000000 ) ;
#2155 = CARTESIAN_POINT ( 'NONE',  ( 4.859338314252994451, 1.606026148912531593, 4.000000000000002665 ) ) ;
#2156 = EDGE_LOOP ( 'NONE', ( #924, #6342 ) ) ;
#2157 = CARTESIAN_POINT ( 'NONE',  ( 5.000000000000001776, 2.886751345948120662, -4.284345921091780696 ) ) ;
#2158 = SURFACE_STYLE_USAGE ( .BOTH. , #3257 ) ;
#2159 = ORIENTED_EDGE ( 'NONE', *, *, #10171, .T. ) ;
#2160 = LINE ( 'NONE', #9912, #410 ) ;
#2161 = VECTOR ( 'NONE', #12396, 1000.000000000000000 ) ;
#2162 = MECHANICAL_DESIGN_GEOMETRIC_PRESENTATION_REPRESENTATION (  '', ( #2391 ), #2881 ) ;
#2163 = DIRECTION ( 'NONE',  ( 1.000000000000000000, 0.000000000000000000, 0.000000000000000000 ) ) ;
#2164 = AXIS2_PLACEMENT_3D ( 'NONE', #9423, #13830, #1366 ) ;
#2165 = ORIENTED_EDGE ( 'NONE', *, *, #4591, .F. ) ;
#2166 = ORIENTED_EDGE ( 'NONE', *, *, #12229, .T. ) ;
#2167 = DIRECTION ( 'NONE',  ( 0.000000000000000000, 0.000000000000000000, 1.000000000000000000 ) ) ;
#2168 = DIRECTION ( 'NONE',  ( 0.000000000000000000, 0.000000000000000000, -1.000000000000000000 ) ) ;
#2169 = CARTESIAN_POINT ( 'NONE',  ( 22.00000000000000000, 78.00000000000000000, -25.00000000000000000 ) ) ;
#2170 = CARTESIAN_POINT ( 'NONE',  ( 59.91362529070399034, 29.57655509336062849, -28.00000000000000000 ) ) ;
#2171 = DIRECTION ( 'NONE',  ( -3.916739600140467622E-15, 1.000000000000000000, 0.000000000000000000 ) ) ;
#2172 = CARTESIAN_POINT ( 'NONE',  ( 4.158921784487740858, 2.089935040870093630, 3.499999999999992006 ) ) ;
#2173 = AXIS2_PLACEMENT_3D ( 'NONE', #3670, #3744, #4828 ) ;
#2174 = VERTEX_POINT ( 'NONE', #7145 ) ;
#2175 = AXIS2_PLACEMENT_3D ( 'NONE', #7594, #1988, #6429 ) ;
#2176 = LINE ( 'NONE', #2096, #3085 ) ;
#2177 = EDGE_CURVE ( 'NONE', #5014, #2858, #3957, .T. ) ;
#2178 = ADVANCED_FACE ( 'NONE', ( #10679 ), #665, .F. ) ;
#2179 = CARTESIAN_POINT ( 'NONE',  ( 4.960798468789972659, 4.316040323963743930, -0.6738506825564518632 ) ) ;
#2180 = CARTESIAN_POINT ( 'NONE',  ( 2.369999999999996998, 0.000000000000000000, 0.000000000000000000 ) ) ;
#2181 = B_SPLINE_CURVE_WITH_KNOTS ( 'NONE', 3,
 ( #2717, #11627, #5267, #1762, #5192, #7382 ),
 .UNSPECIFIED., .F., .F.,
 ( 4, 2, 4 ),
 ( 0.002452478801916370670, 0.003676905084148003947, 0.004901331366379637657 ),
 .UNSPECIFIED. ) ;
#2182 = ORIENTED_EDGE ( 'NONE', *, *, #3874, .T. ) ;
#2183 = ORIENTED_EDGE ( 'NONE', *, *, #13023, .T. ) ;
#2184 = CIRCLE ( 'NONE', #4525, 2.100000000000000977 ) ;
#2185 = ORIENTED_EDGE ( 'NONE', *, *, #3297, .F. ) ;
#2186 = DIRECTION ( 'NONE',  ( -1.000000000000000000, 2.551526159633733968E-19, 1.987661601597216239E-18 ) ) ;
#2187 = EDGE_CURVE ( 'NONE', #2424, #6911, #12850, .T. ) ;
#2188 = ORIENTED_EDGE ( 'NONE', *, *, #3988, .F. ) ;
#2189 = CARTESIAN_POINT ( 'NONE',  ( 0.000000000000000000, 249.5765550933606391, 8.000000000000003553 ) ) ;
#2190 = DIRECTION ( 'NONE',  ( -0.000000000000000000, -1.000000000000000000, -0.000000000000000000 ) ) ;
#2191 = FACE_OUTER_BOUND ( 'NONE', #4724, .T. ) ;
#2192 = CARTESIAN_POINT ( 'NONE',  ( 28.00000000000000355, 29.99999999999999645, 6.999999999999992006 ) ) ;
#2193 = DIRECTION ( 'NONE',  ( -1.000000000000000000, 0.000000000000000000, 0.000000000000000000 ) ) ;
#2194 = EDGE_CURVE ( 'NONE', #11372, #8941, #9136, .T. ) ;
#2195 = CARTESIAN_POINT ( 'NONE',  ( 0.000000000000000000, 40.49999999999999289, 0.000000000000000000 ) ) ;
#2196 = DIRECTION ( 'NONE',  ( 0.000000000000000000, 0.000000000000000000, -1.000000000000000000 ) ) ;
#2197 = CONICAL_SURFACE ( 'NONE', #4080, 4.000000000000000000, 0.8911886515913775009 ) ;
#2198 = EDGE_LOOP ( 'NONE', ( #6287, #12200, #2341, #9735 ) ) ;
#2199 = CARTESIAN_POINT ( 'NONE',  ( 33.99999999999998579, 80.00000000000000000, -23.00000000000000000 ) ) ;
#2200 = ORIENTED_EDGE ( 'NONE', *, *, #5207, .T. ) ;
#2201 = EDGE_LOOP ( 'NONE', ( #2271, #6042, #266, #5597 ) ) ;
#2202 = ORIENTED_EDGE ( 'NONE', *, *, #13155, .T. ) ;
#2203 = AXIS2_PLACEMENT_3D ( 'NONE', #7229, #10389, #3887 ) ;
#2204 = ORIENTED_EDGE ( 'NONE', *, *, #8603, .T. ) ;
#2205 = EDGE_CURVE ( 'NONE', #4466, #1781, #5262, .T. ) ;
#2206 = EDGE_LOOP ( 'NONE', ( #1087, #5917 ) ) ;
#2207 = DIRECTION ( 'NONE',  ( 1.000000000000000000, 0.000000000000000000, 0.000000000000000000 ) ) ;
#2208 =( NAMED_UNIT ( * ) PLANE_ANGLE_UNIT ( ) SI_UNIT ( $, .RADIAN. ) );
#2209 = CARTESIAN_POINT ( 'NONE',  ( 6.136753702857403984E-16, 3.660093687634858650, 1.660531772554304952 ) ) ;
#2210 = ORIENTED_EDGE ( 'NONE', *, *, #4596, .T. ) ;
#2211 = CARTESIAN_POINT ( 'NONE',  ( 18.68170757442808849, 141.2731697022877313, 23.00000000000000000 ) ) ;
#2212 = CARTESIAN_POINT ( 'NONE',  ( 6.800000000000028244, 2.309401076758498039, 4.000000000000003553 ) ) ;
#2214 = VECTOR ( 'NONE', #1061, 1000.000000000000000 ) ;
#2213 = DIRECTION ( 'NONE',  ( -1.000000000000000000, -5.046468293750711996E-16, -1.680811587828860421E-31 ) ) ;
#2215 = CARTESIAN_POINT ( 'NONE',  ( -3.999999999999996447, 2.309401076758494487, -3.133295621305376422 ) ) ;
#2216 = VERTEX_POINT ( 'NONE', #3151 ) ;
#2217 = ORIENTED_EDGE ( 'NONE', *, *, #13988, .T. ) ;
#2218 = DIRECTION ( 'NONE',  ( 1.000000000000000000, 0.000000000000000000, 0.000000000000000000 ) ) ;
#2219 = CARTESIAN_POINT ( 'NONE',  ( 0.000000000000000000, -20.42344490663941414, -33.00000000000000000 ) ) ;
#2220 = CARTESIAN_POINT ( 'NONE',  ( 12.50000000000002132, 12.49999999999999289, -25.00000000000000000 ) ) ;
#2221 = CARTESIAN_POINT ( 'NONE',  ( 20.00000000000000000, -5.510910596163090344E-15, 25.00000000000000000 ) ) ;
#2222 = EDGE_CURVE ( 'NONE', #8618, #6890, #10004, .T. ) ;
#2223 = EDGE_CURVE ( 'NONE', #4126, #4373, #13031, .T. ) ;
#2224 = CARTESIAN_POINT ( 'NONE',  ( 64.10657227073433262, 3.881474981106830757, 25.00000000000000000 ) ) ;
#2225 = CARTESIAN_POINT ( 'NONE',  ( -2.500000000000000444, 3.775608651740452848E-15, -6.000000000000005329 ) ) ;
#2226 = DIRECTION ( 'NONE',  ( 0.000000000000000000, 1.000000000000000000, 0.000000000000000000 ) ) ;
#2227 = CARTESIAN_POINT ( 'NONE',  ( 4.873338085004320419, -0.8268058653460038654, 4.072408605319526309 ) ) ;
#2228 = VERTEX_POINT ( 'NONE', #6632 ) ;
#2229 = EDGE_LOOP ( 'NONE', ( #1714, #13927, #11939, #1969 ) ) ;
#2230 = CARTESIAN_POINT ( 'NONE',  ( 56.75585977000769589, 23.28432498401347672, -25.00000000000000000 ) ) ;
#2231 = ORIENTED_EDGE ( 'NONE', *, *, #2064, .F. ) ;
#2232 = FACE_OUTER_BOUND ( 'NONE', #11849, .T. ) ;
#2233 = ORIENTED_EDGE ( 'NONE', *, *, #7103, .F. ) ;
#2234 = EDGE_CURVE ( 'NONE', #5517, #6626, #9936, .T. ) ;
#2235 = ORIENTED_EDGE ( 'NONE', *, *, #13324, .F. ) ;
#2236 = DIRECTION ( 'NONE',  ( 1.000000000000000000, -2.312964634635743450E-16, -0.000000000000000000 ) ) ;
#2237 = CARTESIAN_POINT ( 'NONE',  ( 51.97979101891770171, 52.38859998837343568, -25.00000000000000000 ) ) ;
#2238 =( REPRESENTATION_RELATIONSHIP ('NONE','NONE', #10295, #2934 ) REPRESENTATION_RELATIONSHIP_WITH_TRANSFORMATION ( #10155 )SHAPE_REPRESENTATION_RELATIONSHIP( ) );
#2239 = DIRECTION ( 'NONE',  ( -1.000000000000000000, 0.000000000000000000, 0.000000000000000000 ) ) ;
#2240 = FACE_BOUND ( 'NONE', #9215, .T. ) ;
#2241 =( LENGTH_UNIT ( ) NAMED_UNIT ( * ) SI_UNIT ( .MILLI., .METRE. ) );
#2242 = CARTESIAN_POINT ( 'NONE',  ( 4.000000000000003553, -2.309401076758511806, -0.5000000000000004441 ) ) ;
#2243 = CARTESIAN_POINT ( 'NONE',  ( 3.951447005078477126, 1.347150628109121673, 3.499999999999996447 ) ) ;
#2244 = EDGE_CURVE ( 'NONE', #10101, #9931, #10957, .T. ) ;
#2245 = ORIENTED_EDGE ( 'NONE', *, *, #6820, .F. ) ;
#2246 = PRESENTATION_STYLE_ASSIGNMENT (( #13299 ) ) ;
#2247 = EDGE_LOOP ( 'NONE', ( #6228, #11523, #8280, #7267 ) ) ;
#2248 = CARTESIAN_POINT ( 'NONE',  ( 3.370256023960729782E-15, 5.773502691896274186, -4.284345921091780696 ) ) ;
#2249 = CARTESIAN_POINT ( 'NONE',  ( 3.065261730689029740, 7.410293710401357536, 8.000000000000007105 ) ) ;
#2250 = VECTOR ( 'NONE', #18, 1000.000000000000000 ) ;
#2251 = EDGE_CURVE ( 'NONE', #2725, #10176, #13782, .T. ) ;
#2252 = ORIENTED_EDGE ( 'NONE', *, *, #3650, .F. ) ;
#2253 = ADVANCED_FACE ( 'NONE', ( #2109 ), #2035, .F. ) ;
#2254 = LINE ( 'NONE', #1220, #4100 ) ;
#2255 = VERTEX_POINT ( 'NONE', #926 ) ;
#2256 = CARTESIAN_POINT ( 'NONE',  ( 22.00000000000000000, 70.00000000000000000, 25.00000000000000000 ) ) ;
#2257 = CARTESIAN_POINT ( 'NONE',  ( 71.80728622811317052, -17.99808865627607801, -25.00000000000000000 ) ) ;
#2258 = EDGE_CURVE ( 'NONE', #5183, #9564, #3081, .T. ) ;
#2259 = FACE_OUTER_BOUND ( 'NONE', #11276, .T. ) ;
#2260 = DIRECTION ( 'NONE',  ( 0.000000000000000000, 0.000000000000000000, 1.000000000000000000 ) ) ;
#2261 = DIRECTION ( 'NONE',  ( 0.9701425001453319874, 0.2425356250363328858, 0.000000000000000000 ) ) ;
#2262 = CARTESIAN_POINT ( 'NONE',  ( 4.197310878070203088, 0.8178547585014672716, -3.202500312981924502 ) ) ;
#2263 = CARTESIAN_POINT ( 'NONE',  ( 22.00000000000000355, 40.00000000000000711, -25.00000000000000000 ) ) ;
#2264 = EDGE_CURVE ( 'NONE', #535, #4153, #3287, .T. ) ;
#2265 = ORIENTED_EDGE ( 'NONE', *, *, #3430, .T. ) ;
#2266 = DIRECTION ( 'NONE',  ( 0.000000000000000000, 0.000000000000000000, -1.000000000000000000 ) ) ;
#2267 = VERTEX_POINT ( 'NONE', #14409 ) ;
#2268 = EDGE_CURVE ( 'NONE', #9459, #1783, #14266, .T. ) ;
#2269 = CARTESIAN_POINT ( 'NONE',  ( -1.257202807339061090, 3.892955774274172054, -3.133250573521038085 ) ) ;
#2270 = VERTEX_POINT ( 'NONE', #7442 ) ;
#2271 = ORIENTED_EDGE ( 'NONE', *, *, #6202, .T. ) ;
#2272 = FACE_OUTER_BOUND ( 'NONE', #2925, .T. ) ;
#2273 = DIRECTION ( 'NONE',  ( 0.000000000000000000, -1.000000000000000000, 0.000000000000000000 ) ) ;
#2274 = DIRECTION ( 'NONE',  ( 0.000000000000000000, 0.000000000000000000, -1.000000000000000000 ) ) ;
#2275 = CARTESIAN_POINT ( 'NONE',  ( 20.00000000000000000, 5.000000000000000000, 25.00000000000000000 ) ) ;
#2276 = CARTESIAN_POINT ( 'NONE',  ( -4.154094228333303107, 2.398367420968265495, -3.421909803043239329 ) ) ;
#2277 = ORIENTED_EDGE ( 'NONE', *, *, #10866, .F. ) ;
#2278 = CARTESIAN_POINT ( 'NONE',  ( -3.549493361947295804E-13, 4.796734841935104576, -3.421909803043237552 ) ) ;
#2279 = ADVANCED_FACE ( 'NONE', ( #7729 ), #9722, .T. ) ;
#2280 = DIRECTION ( 'NONE',  ( -1.000000000000000000, 0.000000000000000000, 0.000000000000000000 ) ) ;
#2281 = DIRECTION ( 'NONE',  ( -1.000000000000000000, 0.000000000000000000, 0.000000000000000000 ) ) ;
#2282 = VECTOR ( 'NONE', #2013, 1000.000000000000114 ) ;
#2283 = DIRECTION ( 'NONE',  ( -0.000000000000000000, -0.000000000000000000, -1.000000000000000000 ) ) ;
#2284 = EDGE_CURVE ( 'NONE', #6358, #9561, #1006, .T. ) ;
#2285 = CARTESIAN_POINT ( 'NONE',  ( 4.966167347451010627, -4.334074124826126528, 0.6428484488894387061 ) ) ;
#2286 = DIRECTION ( 'NONE',  ( 0.000000000000000000, -8.482162385747133845E-47, 1.000000000000000000 ) ) ;
#2287 = CARTESIAN_POINT ( 'NONE',  ( 20.00000000000000000, 27.00000000000000355, 25.00000000000000000 ) ) ;
#2288 =( LENGTH_UNIT ( ) NAMED_UNIT ( * ) SI_UNIT ( .MILLI., .METRE. ) );
#2289 = CIRCLE ( 'NONE', #8370, 5.499999999999976907 ) ;
#2290 = CARTESIAN_POINT ( 'NONE',  ( 5.084394237956035845, 2.335963250529163204, 4.046007034530258117 ) ) ;
#2291 = AXIS2_PLACEMENT_3D ( 'NONE', #13312, #5264, #4182 ) ;
#2292 = EDGE_LOOP ( 'NONE', ( #3899, #7819, #12147, #238, #10818 ) ) ;
#2293 = CARTESIAN_POINT ( 'NONE',  ( 3.951447005078475350, -2.357513599190963927, -2.916666666666674512 ) ) ;
#2294 = EDGE_CURVE ( 'NONE', #2086, #13783, #9869, .T. ) ;
#2295 = ORIENTED_EDGE ( 'NONE', *, *, #13368, .F. ) ;
#2296 = CYLINDRICAL_SURFACE ( 'NONE', #3123, 4.000000000000001776 ) ;
#2297 = ORIENTED_EDGE ( 'NONE', *, *, #7367, .F. ) ;
#2298 = AXIS2_PLACEMENT_3D ( 'NONE', #3726, #502, #4960 ) ;
#2299 = ORIENTED_EDGE ( 'NONE', *, *, #1535, .F. ) ;
#2300 = AXIS2_PLACEMENT_3D ( 'NONE', #4455, #4652, #9995 ) ;
#2301 = DIRECTION ( 'NONE',  ( 0.000000000000000000, -8.482162385747133845E-47, 1.000000000000000000 ) ) ;
#2302 = CARTESIAN_POINT ( 'NONE',  ( 35.00229726637439143, 120.2985749985466839, -25.00000000000000000 ) ) ;
#2303 = CIRCLE ( 'NONE', #6487, 2.499999999999999112 ) ;
#2304 = CARTESIAN_POINT ( 'NONE',  ( 3.972066048304813801, -3.435565134476607163, -1.180968096049836769 ) ) ;
#2305 = PLANE ( 'NONE',  #12341 ) ;
#2306 = DIRECTION ( 'NONE',  ( -2.273843122241288438E-18, -5.551115123125783935E-17, -1.000000000000000000 ) ) ;
#2307 = LINE ( 'NONE', #10060, #4427 ) ;
#2308 = DIRECTION ( 'NONE',  ( -0.000000000000000000, -8.482162385747133845E-47, 1.000000000000000000 ) ) ;
#2309 = ORIENTED_EDGE ( 'NONE', *, *, #14188, .F. ) ;
#2310 = LINE ( 'NONE', #2025, #3690 ) ;
#2311 = EDGE_CURVE ( 'NONE', #5760, #13538, #5795, .T. ) ;
#2312 = EDGE_CURVE ( 'NONE', #6145, #3032, #9788, .T. ) ;
#2313 = B_SPLINE_CURVE_WITH_KNOTS ( 'NONE', 3,
 ( #13775, #10460, #11630, #10175, #156, #9068 ),
 .UNSPECIFIED., .F., .F.,
 ( 4, 2, 4 ),
 ( 0.002336974151641542548, 0.003500975885716412026, 0.004664977619791281505 ),
 .UNSPECIFIED. ) ;
#2314 = LINE ( 'NONE', #4532, #1323 ) ;
#2315 = ORIENTED_EDGE ( 'NONE', *, *, #8603, .F. ) ;
#2316 = VERTEX_POINT ( 'NONE', #8252 ) ;
#2317 = ORIENTED_EDGE ( 'NONE', *, *, #11197, .F. ) ;
#2318 = DIRECTION ( 'NONE',  ( 0.000000000000000000, 0.000000000000000000, 1.000000000000000000 ) ) ;
#2319 = B_SPLINE_CURVE_WITH_KNOTS ( 'NONE', 3,
 ( #2375, #4451, #13507, #6534, #4647 ),
 .UNSPECIFIED., .F., .F.,
 ( 4, 1, 4 ),
 ( 0.000000000000000000, 0.002020725942163693108, 0.004041451884327386217 ),
 .UNSPECIFIED. ) ;
#2320 = VERTEX_POINT ( 'NONE', #13178 ) ;
#2321 = LINE ( 'NONE', #5533, #13804 ) ;
#2322 = VECTOR ( 'NONE', #4576, 1000.000000000000000 ) ;
#2323 = CARTESIAN_POINT ( 'NONE',  ( 5.000000000000001776, -3.130589478369270928, -4.327780579809764383 ) ) ;
#2324 = LINE ( 'NONE', #6775, #12846 ) ;
#2325 = PLANE ( 'NONE',  #5561 ) ;
#2326 = CARTESIAN_POINT ( 'NONE',  ( 60.00000000000000000, -6.123233995736768255E-16, -25.00000000000000000 ) ) ;
#2327 = VECTOR ( 'NONE', #2940, 1000.000000000000000 ) ;
#2328 = CARTESIAN_POINT ( 'NONE',  ( 2.500000000000011546, -4.330127018922186544, 0.000000000000000000 ) ) ;
#2329 = CARTESIAN_POINT ( 'NONE',  ( 3.878096787214413421, -2.680238624820956872, 2.357690525401561210 ) ) ;
#2330 = CARTESIAN_POINT ( 'NONE',  ( 71.80728622811317052, -17.99808865627607801, -25.00000000000000000 ) ) ;
#2331 = VECTOR ( 'NONE', #11780, 1000.000000000000000 ) ;
#2332 = ORIENTED_EDGE ( 'NONE', *, *, #7478, .T. ) ;
#2333 = AXIS2_PLACEMENT_3D ( 'NONE', #14004, #2053, #4343 ) ;
#2334 = CARTESIAN_POINT ( 'NONE',  ( 2.750000000000003997, 40.49999999999999289, 8.000000000000007105 ) ) ;
#2335 = EDGE_LOOP ( 'NONE', ( #2309, #9256 ) ) ;
#2336 = ORIENTED_EDGE ( 'NONE', *, *, #3180, .T. ) ;
#2337 = CARTESIAN_POINT ( 'NONE',  ( 1.738521435313293395, -5.045405839192998343, -4.385926550512764699 ) ) ;
#2338 = DIRECTION ( 'NONE',  ( 1.000000000000000000, 1.665334536937734318E-16, 0.000000000000000000 ) ) ;
#2339 = ADVANCED_FACE ( 'NONE', ( #7581, #14338 ), #1150, .T. ) ;
#2340 = CARTESIAN_POINT ( 'NONE',  ( 92.68170757442806007, 124.5765550933605965, 25.00000000000000000 ) ) ;
#2341 = ORIENTED_EDGE ( 'NONE', *, *, #7099, .F. ) ;
#2342 = CARTESIAN_POINT ( 'NONE',  ( 0.000000000000000000, 0.000000000000000000, -25.00000000000000000 ) ) ;
#2343 = AXIS2_PLACEMENT_3D ( 'NONE', #12678, #12529, #13580 ) ;
#2344 = CARTESIAN_POINT ( 'NONE',  ( 108.6817075744280174, 69.57655509336049704, -3.299999999999981171 ) ) ;
#2345 = DIRECTION ( 'NONE',  ( -1.000000000000000000, 0.000000000000000000, 0.000000000000000000 ) ) ;
#2346 = CARTESIAN_POINT ( 'NONE',  ( 28.00000000000000355, 29.99999999999999645, -25.00000000000000000 ) ) ;
#2347 = ORIENTED_EDGE ( 'NONE', *, *, #194, .T. ) ;
#2348 = EDGE_CURVE ( 'NONE', #8916, #9931, #10213, .T. ) ;
#2349 = EDGE_CURVE ( 'NONE', #1777, #8228, #9032, .T. ) ;
#2350 = DIRECTION ( 'NONE',  ( -0.000000000000000000, 1.000000000000000000, -0.000000000000000000 ) ) ;
#2351 = DIRECTION ( 'NONE',  ( 0.000000000000000000, 0.000000000000000000, 1.000000000000000000 ) ) ;
#2352 = COLOUR_RGB ( '', 0.72549020, 0.75294118, 0.79215686) ;
#2353 = ORIENTED_EDGE ( 'NONE', *, *, #6759, .T. ) ;
#2354 =( BOUNDED_SURFACE ( )  B_SPLINE_SURFACE ( 3, 2, ( 
 ( #12419, #3429, #5469 ),
 ( #5396, #1004, #6630 ),
 ( #9865, #3212, #5602 ),
 ( #13392, #13460, #2394 ),
 ( #5672, #7872, #10074 ),
 ( #8827, #13309, #8760 ) ),
 .UNSPECIFIED., .F., .F., .T. ) 
 B_SPLINE_SURFACE_WITH_KNOTS ( ( 4, 2, 4 ),
 ( 3, 3 ),
 ( 0.01652267773200353021, 0.01858309280828997906, 0.02064350788457643138 ),
 ( 0.000000000000000000, 1.000000000000000000 ),
 .UNSPECIFIED. ) 
 GEOMETRIC_REPRESENTATION_ITEM ( )  RATIONAL_B_SPLINE_SURFACE ( (
 ( 1.000000000000000000, 0.8047780975688292315, 1.000000000000000000),
 ( 1.000000000000000000, 0.8123789546319812871, 1.000000000000000000),
 ( 1.000000000000000000, 0.8190677982995108186, 1.000000000000000000),
 ( 1.000000000000000000, 0.8192346069545793918, 1.000000000000000000),
 ( 1.000000000000000000, 0.8126126759773680819, 1.000000000000000000),
 ( 1.000000000000000000, 0.8047712639311999094, 1.000000000000000000) ) ) 
 REPRESENTATION_ITEM ( '' )  SURFACE ( )  );
#2355 = AXIS2_PLACEMENT_3D ( 'NONE', #2146, #958, #12091 ) ;
#2356 = CARTESIAN_POINT ( 'NONE',  ( 4.870920456765270856, -3.129869081975100276, 2.723603336645685769 ) ) ;
#2357 = CARTESIAN_POINT ( 'NONE',  ( 4.050880675075964277, -1.379097446046169795, -3.567934390854442306 ) ) ;
#2358 = EDGE_CURVE ( 'NONE', #9831, #10243, #11943, .T. ) ;
#2359 = EDGE_CURVE ( 'NONE', #8228, #11273, #5310, .T. ) ;
#2360 = DIRECTION ( 'NONE',  ( -0.3822382184081050127, -0.9240638205168504316, 0.000000000000000000 ) ) ;
#2361 = SURFACE_STYLE_USAGE ( .BOTH. , #7982 ) ;
#2362 = VECTOR ( 'NONE', #9044, 1000.000000000000000 ) ;
#2363 = CARTESIAN_POINT ( 'NONE',  ( 5.103279350327357911, 2.353751664345929306, 4.076817471046935815 ) ) ;
#2364 = ORIENTED_EDGE ( 'NONE', *, *, #11159, .T. ) ;
#2365 = AXIS2_PLACEMENT_3D ( 'NONE', #14253, #2308, #14397 ) ;
#2366 = CARTESIAN_POINT ( 'NONE',  ( -4.197393957002300446, -0.8151795401431400911, -3.203767560748917553 ) ) ;
#2367 = VECTOR ( 'NONE', #2283, 1000.000000000000000 ) ;
#2368 =( LENGTH_UNIT ( ) NAMED_UNIT ( * ) SI_UNIT ( .MILLI., .METRE. ) );
#2369 = EDGE_LOOP ( 'NONE', ( #9647, #9703, #2381, #4239, #3780, #506 ) ) ;
#2370 = CARTESIAN_POINT ( 'NONE',  ( 64.10657227073433262, 3.881474981106830757, -25.00000000000000000 ) ) ;
#2371 = AXIS2_PLACEMENT_3D ( 'NONE', #11928, #6421, #14269 ) ;
#2372 = STYLED_ITEM ( 'NONE', ( #7456 ), #11496 ) ;
#2373 = VECTOR ( 'NONE', #5556, 1000.000000000000000 ) ;
#2374 = LINE ( 'NONE', #3482, #2214 ) ;
#2375 = CARTESIAN_POINT ( 'NONE',  ( 4.071447262713911996, -4.041451884327377009, 0.000000000000000000 ) ) ;
#2376 = EDGE_CURVE ( 'NONE', #9459, #11964, #1358, .T. ) ;
#2377 = CARTESIAN_POINT ( 'NONE',  ( 22.00000000000000355, 30.00000000000000711, 25.00000000000000000 ) ) ;
#2378 = CARTESIAN_POINT ( 'NONE',  ( 20.00000000000000000, 37.00000000000000711, 25.00000000000000000 ) ) ;
#2379 = LINE ( 'NONE', #4720, #7432 ) ;
#2380 = DIRECTION ( 'NONE',  ( -0.000000000000000000, -0.000000000000000000, -1.000000000000000000 ) ) ;
#2381 = ORIENTED_EDGE ( 'NONE', *, *, #2115, .F. ) ;
#2382 = LINE ( 'NONE', #12536, #10066 ) ;
#2383 = ORIENTED_EDGE ( 'NONE', *, *, #5122, .F. ) ;
#2384 = CARTESIAN_POINT ( 'NONE',  ( -3.999999999999996447, -1.560351142792946399, -0.2242961665059788057 ) ) ;
#2385 = AXIS2_PLACEMENT_3D ( 'NONE', #6992, #10437, #8307 ) ;
#2386 = AXIS2_PLACEMENT_3D ( 'NONE', #9727, #11705, #9515 ) ;
#2387 = CARTESIAN_POINT ( 'NONE',  ( 1.560000000000005826, -1.732050807568885631, 0.000000000000000000 ) ) ;
#2388 = EDGE_LOOP ( 'NONE', ( #8972, #10139, #12616, #7615, #6326 ) ) ;
#2389 = ORIENTED_EDGE ( 'NONE', *, *, #9189, .F. ) ;
#2390 = CARTESIAN_POINT ( 'NONE',  ( 0.000000000000000000, 2.081668171172168513E-14, 4.000000000000003553 ) ) ;
#2391 = STYLED_ITEM ( 'NONE', ( #250 ), #14323 ) ;
#2392 = EDGE_CURVE ( 'NONE', #11916, #5464, #3580, .T. ) ;
#2393 = EDGE_LOOP ( 'NONE', ( #9202, #2609, #2185, #9680 ) ) ;
#2394 = CARTESIAN_POINT ( 'NONE',  ( 3.972073812946703253, -0.6951863858504719884, -3.565770933504595952 ) ) ;
#2395 = AXIS2_PLACEMENT_3D ( 'NONE', #1692, #11792, #526 ) ;
#2396 = PRODUCT_RELATED_PRODUCT_CATEGORY ( 'part', '', ( #13505 ) ) ;
#2397 = EDGE_CURVE ( 'NONE', #260, #5200, #8016, .T. ) ;
#2398 = CARTESIAN_POINT ( 'NONE',  ( 6.250000000000033751, 9.714451465470119729E-15, 6.249999999999993783 ) ) ;
#2399 = DIRECTION ( 'NONE',  ( 1.000000000000000000, 0.000000000000000000, 0.000000000000000000 ) ) ;
#2400 = LINE ( 'NONE', #3434, #11888 ) ;
#2401 = CARTESIAN_POINT ( 'NONE',  ( 2.500000000000002220, 4.163336342344338999E-16, -4.699999999999981526 ) ) ;
#2402 = DIRECTION ( 'NONE',  ( 0.000000000000000000, 0.000000000000000000, 1.000000000000000000 ) ) ;
#2403 = CARTESIAN_POINT ( 'NONE',  ( 4.960411150172048700, -1.572332708191213291, 4.074718599813436093 ) ) ;
#2404 = CARTESIAN_POINT ( 'NONE',  ( 5.056385618527004411, -4.642911450026661058, -1.387778780781445676E-14 ) ) ;
#2405 = PRESENTATION_LAYER_ASSIGNMENT (  '', '', ( #7530 ) ) ;
#2406 = AXIS2_PLACEMENT_3D ( 'NONE', #13405, #9944, #14349 ) ;
#2407 = ORIENTED_EDGE ( 'NONE', *, *, #820, .F. ) ;
#2408 = CARTESIAN_POINT ( 'NONE',  ( -4.141042022537586575, 2.227970427079376314, -3.387027626239150546 ) ) ;
#2409 = EDGE_LOOP ( 'NONE', ( #7696, #2977, #9012, #13717 ) ) ;
#2410 = DIRECTION ( 'NONE',  ( -0.000000000000000000, -0.000000000000000000, 1.000000000000000000 ) ) ;
#2411 = EDGE_CURVE ( 'NONE', #6243, #549, #10151, .T. ) ;
#2412 = CARTESIAN_POINT ( 'NONE',  ( 118.6817075744280174, -20.42344490663938927, 33.00000000000002842 ) ) ;
#2413 = LINE ( 'NONE', #11334, #457 ) ;
#2414 = DIRECTION ( 'NONE',  ( -1.000000000000000000, 0.000000000000000000, 0.000000000000000000 ) ) ;
#2415 = AXIS2_PLACEMENT_3D ( 'NONE', #14438, #12160, #9966 ) ;
#2416 = EDGE_LOOP ( 'NONE', ( #10027, #9998, #5074, #10285, #11594 ) ) ;
#2417 = DIRECTION ( 'NONE',  ( 0.000000000000000000, 0.000000000000000000, -1.000000000000000000 ) ) ;
#2418 = CARTESIAN_POINT ( 'NONE',  ( -125.4817075744280572, 69.57655509336046862, 1.912698017079632571E-14 ) ) ;
#2419 = DIRECTION ( 'NONE',  ( 0.000000000000000000, 0.000000000000000000, 1.000000000000000000 ) ) ;
#2420 = ORIENTED_EDGE ( 'NONE', *, *, #8347, .T. ) ;
#2421 = VECTOR ( 'NONE', #11545, 1000.000000000000000 ) ;
#2422 = DIRECTION ( 'NONE',  ( 0.000000000000000000, 0.000000000000000000, 1.000000000000000000 ) ) ;
#2423 = AXIS2_PLACEMENT_3D ( 'NONE', #6656, #11125, #2345 ) ;
#2424 = VERTEX_POINT ( 'NONE', #6774 ) ;
#2425 = ORIENTED_EDGE ( 'NONE', *, *, #8136, .F. ) ;
#2426 = VECTOR ( 'NONE', #5088, 1000.000000000000000 ) ;
#2427 = ADVANCED_FACE ( 'NONE', ( #11319 ), #4044, .F. ) ;
#2428 = CYLINDRICAL_SURFACE ( 'NONE', #13729, 2.500000000000002220 ) ;
#2429 = DIRECTION ( 'NONE',  ( 0.000000000000000000, 1.000000000000000000, 0.000000000000000000 ) ) ;
#2430 = SURFACE_SIDE_STYLE ('',( #5840 ) ) ;
#2431 = EDGE_CURVE ( 'NONE', #2216, #6532, #8082, .T. ) ;
#2432 = EDGE_LOOP ( 'NONE', ( #6062, #4963, #12979 ) ) ;
#2433 = DIRECTION ( 'NONE',  ( -0.000000000000000000, 0.000000000000000000, 1.000000000000000000 ) ) ;
#2434 = DIRECTION ( 'NONE',  ( -0.9396926207859144231, -1.564902575500316617E-16, -0.3420201433256524481 ) ) ;
#2435 = ORIENTED_EDGE ( 'NONE', *, *, #14124, .T. ) ;
#2436 = CLOSED_SHELL ( 'NONE', ( #7622, #13352, #7363, #5558, #4052, #5478, #8462, #6175, #12674, #5272, #963, #11640, #12561, #4775, #9859, #8044, #701, #5129, #7603, #10411, #5256, #811, #12606, #7549, #577, #12763, #2611, #6091, #4267, #9409, #7704, #10797, #9868, #264, #11833, #12856, #10203, #12636, #4124, #8382, #10124, #11221, #3466, #1015, #8733, #8910, #195 ) ) ;
#2437 = ADVANCED_FACE ( 'NONE', ( #4468 ), #168, .F. ) ;
#2438 = CARTESIAN_POINT ( 'NONE',  ( -140.0000000000003411, 199.5765550933606107, -132.0000000000000000 ) ) ;
#2439 = ORIENTED_EDGE ( 'NONE', *, *, #5332, .T. ) ;
#2440 = EDGE_LOOP ( 'NONE', ( #7449, #6177, #2217, #11767 ) ) ;
#2441 = ADVANCED_FACE ( 'NONE', ( #10367 ), #8373, .T. ) ;
#2442 = DIRECTION ( 'NONE',  ( -1.000000000000000000, 0.000000000000000000, 0.000000000000000000 ) ) ;
#2443 = CARTESIAN_POINT ( 'NONE',  ( 4.175075985190068728, 2.060370777630132544, 3.568666869285544330 ) ) ;
#2444 = CARTESIAN_POINT ( 'NONE',  ( 4.114405500665256454, -2.025575754679707519, -3.508400121684932760 ) ) ;
#2445 = DIRECTION ( 'NONE',  ( 1.000000000000000000, 0.000000000000000000, 0.000000000000000000 ) ) ;
#2446 = SHAPE_REPRESENTATION_RELATIONSHIP ( 'NONE' , 'NONE' ,  #852, #6268 ) ;
#2447 = DIRECTION ( 'NONE',  ( -1.000000000000000000, 0.000000000000000000, 0.000000000000000000 ) ) ;
#2448 = ORIENTED_EDGE ( 'NONE', *, *, #6615, .F. ) ;
#2449 = VECTOR ( 'NONE', #13472, 1000.000000000000000 ) ;
#2450 = CARTESIAN_POINT ( 'NONE',  ( 5.103531824934115946, 2.354098498486452584, 4.077418205400126894 ) ) ;
#2451 = ORIENTED_EDGE ( 'NONE', *, *, #10501, .T. ) ;
#2452 = DIRECTION ( 'NONE',  ( 1.000000000000000000, 1.665334536937734318E-16, 0.000000000000000000 ) ) ;
#2453 = EDGE_LOOP ( 'NONE', ( #7931, #9555, #808, #10717 ) ) ;
#2454 = CARTESIAN_POINT ( 'NONE',  ( 60.00000000000000000, -6.123233995736768255E-16, -25.00000000000000000 ) ) ;
#2455 = ORIENTED_EDGE ( 'NONE', *, *, #12096, .F. ) ;
#2456 = CARTESIAN_POINT ( 'NONE',  ( 2.949999999999994404, 0.000000000000000000, 0.000000000000000000 ) ) ;
#2457 = AXIS2_PLACEMENT_3D ( 'NONE', #2670, #1636, #12530 ) ;
#2458 = ADVANCED_FACE ( 'NONE', ( #11171 ), #6259, .T. ) ;
#2459 = VERTEX_POINT ( 'NONE', #574 ) ;
#2460 = VECTOR ( 'NONE', #13939, 1000.000000000000000 ) ;
#2461 = EDGE_LOOP ( 'NONE', ( #5924, #11778, #11236, #6216, #155 ) ) ;
#2462 = ORIENTED_EDGE ( 'NONE', *, *, #5881, .T. ) ;
#2463 = CARTESIAN_POINT ( 'NONE',  ( 1.210692425942146947E-15, -0.3908539631355372190, -4.000000000000004441 ) ) ;
#2464 = EDGE_CURVE ( 'NONE', #2174, #9318, #9566, .T. ) ;
#2465 = CARTESIAN_POINT ( 'NONE',  ( 1.560000000000005826, -1.732050807568885631, 0.000000000000000000 ) ) ;
#2466 = CARTESIAN_POINT ( 'NONE',  ( 5.000000000000001776, -1.069734140705724146, -4.273127864870867931 ) ) ;
#2467 = DIRECTION ( 'NONE',  ( -0.000000000000000000, 0.000000000000000000, -1.000000000000000000 ) ) ;
#2468 = CARTESIAN_POINT ( 'NONE',  ( 2.369999999999996998, 0.000000000000000000, 0.000000000000000000 ) ) ;
#2469 = ORIENTED_EDGE ( 'NONE', *, *, #2475, .F. ) ;
#2470 = LINE ( 'NONE', #2546, #4243 ) ;
#2471 = LINE ( 'NONE', #13614, #2362 ) ;
#2473 = VECTOR ( 'NONE', #2726, 1000.000000000000114 ) ;
#2472 = CARTESIAN_POINT ( 'NONE',  ( -4.197477404309741367, 0.8522071663317644097, -3.205040426610007209 ) ) ;
#2474 = LINE ( 'NONE', #6923, #10329 ) ;
#2475 = EDGE_CURVE ( 'NONE', #3711, #3862, #12776, .T. ) ;
#2476 = ORIENTED_EDGE ( 'NONE', *, *, #13211, .F. ) ;
#2477 = CARTESIAN_POINT ( 'NONE',  ( 118.6817075744280316, 69.57655509336046862, -3.299999999999976730 ) ) ;
#2478 = EDGE_LOOP ( 'NONE', ( #4965, #2705, #11804, #1067 ) ) ;
#2479 = CARTESIAN_POINT ( 'NONE',  ( 44.62907851819101523, 71.79144999128007498, -25.00000000000000000 ) ) ;
#2480 = CARTESIAN_POINT ( 'NONE',  ( 22.00000000000000000, 70.00000000000000000, -25.00000000000000000 ) ) ;
#2481 = DIRECTION ( 'NONE',  ( 1.000000000000000000, 0.000000000000000000, 0.000000000000000000 ) ) ;
#2482 = CARTESIAN_POINT ( 'NONE',  ( -5.000000000000000000, 2.886751345948124214, -0.5999999999999894307 ) ) ;
#2483 = VERTEX_POINT ( 'NONE', #1658 ) ;
#2484 = PLANE ( 'NONE',  #4019 ) ;
#2485 = DIRECTION ( 'NONE',  ( 0.9237280213470682178, 0.3830490080632377725, 0.000000000000000000 ) ) ;
#2486 = DIRECTION ( 'NONE',  ( -1.000000000000000000, 2.551526159633717598E-19, -1.734723475976770887E-18 ) ) ;
#2487 = EDGE_CURVE ( 'NONE', #14260, #13012, #1468, .T. ) ;
#2488 = EDGE_CURVE ( 'NONE', #12697, #2567, #2075, .T. ) ;
#2489 = CARTESIAN_POINT ( 'NONE',  ( 20.00000000000000355, 50.00000000000000000, 25.00000000000000000 ) ) ;
#2490 = ORIENTED_EDGE ( 'NONE', *, *, #13049, .F. ) ;
#2491 = AXIS2_PLACEMENT_3D ( 'NONE', #8792, #9971, #5638 ) ;
#2492 = EDGE_LOOP ( 'NONE', ( #3472, #7425, #6478, #3054 ) ) ;
#2493 = ORIENTED_EDGE ( 'NONE', *, *, #10301, .F. ) ;
#2494 = EDGE_CURVE ( 'NONE', #10570, #5783, #6675, .T. ) ;
#2495 = DIRECTION ( 'NONE',  ( 3.286707217423841172E-17, 1.000000000000000000, -5.551115123125782702E-17 ) ) ;
#2496 = DIRECTION ( 'NONE',  ( 0.000000000000000000, 0.000000000000000000, -1.000000000000000000 ) ) ;
#2497 = ORIENTED_EDGE ( 'NONE', *, *, #9688, .T. ) ;
#2498 = ORIENTED_EDGE ( 'NONE', *, *, #7318, .T. ) ;
#2499 = FACE_OUTER_BOUND ( 'NONE', #13157, .T. ) ;
#2500 = AXIS2_PLACEMENT_3D ( 'NONE', #13365, #11609, #5811 ) ;
#2501 = EDGE_CURVE ( 'NONE', #7349, #8967, #4648, .T. ) ;
#2502 = FACE_BOUND ( 'NONE', #6506, .T. ) ;
#2503 = EDGE_CURVE ( 'NONE', #2898, #7089, #7209, .T. ) ;
#2504 = VERTEX_POINT ( 'NONE', #3867 ) ;
#2505 = FACE_OUTER_BOUND ( 'NONE', #5939, .T. ) ;
#2506 = B_SPLINE_CURVE_WITH_KNOTS ( 'NONE', 3,
 ( #8565, #1918, #2880, #6064, #7324, #3969 ),
 .UNSPECIFIED., .F., .F.,
 ( 4, 2, 4 ),
 ( 0.005852013098461913629, 0.006875955139453155188, 0.007899897180444396746 ),
 .UNSPECIFIED. ) ;
#2507 = PRODUCT_DEFINITION_SHAPE ( 'NONE', 'NONE',  #6941 ) ;
#2508 = EDGE_CURVE ( 'NONE', #7523, #2748, #8301, .T. ) ;
#2509 = CARTESIAN_POINT ( 'NONE',  ( 0.03458865240596911694, 0.7871057074556094824, -4.000000000000003553 ) ) ;
#2510 = DIRECTION ( 'NONE',  ( 1.000000000000000000, 8.619211990076297369E-16, 0.000000000000000000 ) ) ;
#2511 = VECTOR ( 'NONE', #3568, 1000.000000000000000 ) ;
#2512 = AXIS2_PLACEMENT_3D ( 'NONE', #7495, #1965, #1665 ) ;
#2513 = CARTESIAN_POINT ( 'NONE',  ( 0.000000000000000000, 0.000000000000000000, -23.00000000000000000 ) ) ;
#2514 = DIRECTION ( 'NONE',  ( 0.000000000000000000, -4.440892098500620245E-16, -1.000000000000000000 ) ) ;
#2515 = EDGE_CURVE ( 'NONE', #4441, #2985, #8459, .T. ) ;
#2516 = DIRECTION ( 'NONE',  ( 0.000000000000000000, 5.551115123125782702E-17, 1.000000000000000000 ) ) ;
#2517 = EDGE_CURVE ( 'NONE', #4300, #2898, #12321, .T. ) ;
#2518 = FACE_OUTER_BOUND ( 'NONE', #7435, .T. ) ;
#2519 = EDGE_LOOP ( 'NONE', ( #13497, #2819, #2761, #13622 ) ) ;
#2520 = DIRECTION ( 'NONE',  ( 0.000000000000000000, 0.000000000000000000, -1.000000000000000000 ) ) ;
#2521 = ORIENTED_EDGE ( 'NONE', *, *, #9187, .T. ) ;
#2522 = DIRECTION ( 'NONE',  ( 0.000000000000000000, 0.000000000000000000, -1.000000000000000000 ) ) ;
#2523 =( BOUNDED_SURFACE ( )  B_SPLINE_SURFACE ( 3, 2, ( 
 ( #12082, #14359, #7670 ),
 ( #6502, #6240, #12923 ),
 ( #11054, #9888, #2056 ),
 ( #10972, #5554, #8849 ),
 ( #947, #4489, #7340 ),
 ( #876, #5488, #11817 ) ),
 .UNSPECIFIED., .F., .F., .T. ) 
 B_SPLINE_SURFACE_WITH_KNOTS ( ( 4, 2, 4 ),
 ( 3, 3 ),
 ( 0.01886032586153034429, 0.02121253401777977582, 0.02356474217402920734 ),
 ( 0.000000000000000000, 1.000000000000000000 ),
 .UNSPECIFIED. ) 
 GEOMETRIC_REPRESENTATION_ITEM ( )  RATIONAL_B_SPLINE_SURFACE ( (
 ( 1.000000000000000000, 0.8047781103519396906, 1.000000000000000000),
 ( 1.000000000000000000, 0.8123785825774894054, 1.000000000000000000),
 ( 1.000000000000000000, 0.8190671539561196202, 1.000000000000000000),
 ( 1.000000000000000000, 0.8192352255061938759, 1.000000000000000000),
 ( 1.000000000000000000, 0.8126129677041067367, 1.000000000000000000),
 ( 1.000000000000000000, 0.8047712537969723412, 1.000000000000000000) ) ) 
 REPRESENTATION_ITEM ( '' )  SURFACE ( )  );
#2524 = DIRECTION ( 'NONE',  ( -1.000000000000000000, 0.000000000000000000, 0.000000000000000000 ) ) ;
#2525 = ADVANCED_FACE ( 'NONE', ( #13822 ), #9745, .T. ) ;
#2526 = ORIENTED_EDGE ( 'NONE', *, *, #4864, .F. ) ;
#2527 = DIRECTION ( 'NONE',  ( -0.2425356250363328581, 0.9701425001453318764, 0.000000000000000000 ) ) ;
#2528 = ADVANCED_FACE ( 'NONE', ( #6107 ), #5028, .F. ) ;
#2529 = VECTOR ( 'NONE', #427, 1000.000000000000000 ) ;
#2530 = VECTOR ( 'NONE', #13377, 1000.000000000000000 ) ;
#2531 = AXIS2_PLACEMENT_3D ( 'NONE', #182, #13379, #12335 ) ;
#2532 = ORIENTED_EDGE ( 'NONE', *, *, #4053, .F. ) ;
#2533 = B_SPLINE_CURVE_WITH_KNOTS ( 'NONE', 3,
 ( #7949, #1364, #10219, #12429, #2548 ),
 .UNSPECIFIED., .F., .F.,
 ( 4, 1, 4 ),
 ( 0.000000000000000000, 0.002020725942163691807, 0.004041451884327383615 ),
 .UNSPECIFIED. ) ;
#2534 = CARTESIAN_POINT ( 'NONE',  ( 0.000000000000000000, 0.000000000000000000, 0.000000000000000000 ) ) ;
#2535 = ORIENTED_EDGE ( 'NONE', *, *, #13933, .F. ) ;
#2536 = FACE_OUTER_BOUND ( 'NONE', #12567, .T. ) ;
#2537 = CARTESIAN_POINT ( 'NONE',  ( -5.551115123125782702E-14, 3.464101615137750390, -2.000000000000001776 ) ) ;
#2538 = ORIENTED_EDGE ( 'NONE', *, *, #13660, .F. ) ;
#2539 = DIRECTION ( 'NONE',  ( -0.000000000000000000, -0.000000000000000000, -1.000000000000000000 ) ) ;
#2540 = DIRECTION ( 'NONE',  ( 0.000000000000000000, 0.000000000000000000, -1.000000000000000000 ) ) ;
#2541 = EDGE_CURVE ( 'NONE', #12769, #7655, #11233, .T. ) ;
#2542 = DIRECTION ( 'NONE',  ( 1.000000000000000000, 0.000000000000000000, 0.000000000000000000 ) ) ;
#2543 = EDGE_CURVE ( 'NONE', #3708, #1484, #11614, .T. ) ;
#2544 = CARTESIAN_POINT ( 'NONE',  ( 6.800000000000028244, 2.309401076758504701, -4.000000000000003553 ) ) ;
#2545 = AXIS2_PLACEMENT_3D ( 'NONE', #1882, #12860, #5093 ) ;
#2546 = CARTESIAN_POINT ( 'NONE',  ( 20.00000000000000355, 30.00000000000000711, 25.00000000000000000 ) ) ;
#2547 = CONTEXT_DEPENDENT_SHAPE_REPRESENTATION ( #458, #13296 ) ;
#2548 = CARTESIAN_POINT ( 'NONE',  ( 4.071447262713911996, 4.041451884327390331, 0.000000000000000000 ) ) ;
#2549 = CARTESIAN_POINT ( 'NONE',  ( 0.3126073911696169993, 2.020725942163681399, 3.499999999999996003 ) ) ;
#2550 = CARTESIAN_POINT ( 'NONE',  ( 5.000000000000000000, -2.886751345948152192, -0.5999999999999894307 ) ) ;
#2551 = ORIENTED_EDGE ( 'NONE', *, *, #3641, .T. ) ;
#2552 = CARTESIAN_POINT ( 'NONE',  ( 0.1750032273043234943, 4.719840313910212082, -3.169254239516200222 ) ) ;
#2553 = ORIENTED_EDGE ( 'NONE', *, *, #356, .F. ) ;
#2554 = VERTEX_POINT ( 'NONE', #2924 ) ;
#2555 = CARTESIAN_POINT ( 'NONE',  ( 0.000000000000000000, 4.618802153517016507, -4.699999999999981526 ) ) ;
#2556 = AXIS2_PLACEMENT_3D ( 'NONE', #8398, #1756, #726 ) ;
#2557 = DIRECTION ( 'NONE',  ( 0.000000000000000000, 0.000000000000000000, -1.000000000000000000 ) ) ;
#2558 = CARTESIAN_POINT ( 'NONE',  ( 20.00000000000000000, 60.00000000000000711, -25.00000000000000000 ) ) ;
#2559 = EDGE_CURVE ( 'NONE', #6341, #10062, #12622, .T. ) ;
#2560 = DIRECTION ( 'NONE',  ( 0.000000000000000000, 0.000000000000000000, -1.000000000000000000 ) ) ;
#2561 = ORIENTED_EDGE ( 'NONE', *, *, #10392, .F. ) ;
#2562 = LINE ( 'NONE', #13698, #6339 ) ;
#2563 = FACE_OUTER_BOUND ( 'NONE', #3025, .T. ) ;
#2564 = CIRCLE ( 'NONE', #3503, 2.699999999999999289 ) ;
#2565 = DIRECTION ( 'NONE',  ( -0.000000000000000000, 1.000000000000000000, -0.000000000000000000 ) ) ;
#2566 =( GEOMETRIC_REPRESENTATION_CONTEXT ( 3 ) GLOBAL_UNCERTAINTY_ASSIGNED_CONTEXT ( ( #6305 ) ) GLOBAL_UNIT_ASSIGNED_CONTEXT ( ( #10838, #2208, #14357 ) ) REPRESENTATION_CONTEXT ( 'NONE', 'WORKASPACE' ) );
#2567 = VERTEX_POINT ( 'NONE', #10432 ) ;
#2568 = ORIENTED_EDGE ( 'NONE', *, *, #1170, .T. ) ;
#2569 = ORIENTED_EDGE ( 'NONE', *, *, #2575, .F. ) ;
#2570 = ORIENTED_EDGE ( 'NONE', *, *, #2223, .F. ) ;
#2571 = CARTESIAN_POINT ( 'NONE',  ( 59.10586122665984732, -20.42344490663941414, 23.00000000000000000 ) ) ;
#2572 = CARTESIAN_POINT ( 'NONE',  ( 76.68170757442798902, 124.5765550933606249, -25.00000000000000000 ) ) ;
#2573 = EDGE_CURVE ( 'NONE', #14451, #716, #9337, .T. ) ;
#2574 = PRODUCT_DEFINITION ( 'UNKNOWN', '', #9674, #3673 ) ;
#2575 = EDGE_CURVE ( 'NONE', #9662, #6876, #5453, .T. ) ;
#2576 =( NAMED_UNIT ( * ) SI_UNIT ( $, .STERADIAN. ) SOLID_ANGLE_UNIT ( ) );
#2577 = ORIENTED_EDGE ( 'NONE', *, *, #8273, .T. ) ;
#2578 = DIRECTION ( 'NONE',  ( -1.000000000000000000, 0.000000000000000000, -0.000000000000000000 ) ) ;
#2579 = CARTESIAN_POINT ( 'NONE',  ( 68.68170757442801744, 29.57655509336062849, -117.0000000000000000 ) ) ;
#2580 = AXIS2_PLACEMENT_3D ( 'NONE', #6611, #8745, #11151 ) ;
#2581 = ORIENTED_EDGE ( 'NONE', *, *, #6981, .T. ) ;
#2582 = DIRECTION ( 'NONE',  ( 0.000000000000000000, 0.000000000000000000, 1.000000000000000000 ) ) ;
#2583 = ORIENTED_EDGE ( 'NONE', *, *, #2706, .T. ) ;
#2584 = FACE_OUTER_BOUND ( 'NONE', #3768, .T. ) ;
#2585 = PLANE ( 'NONE',  #1953 ) ;
#2586 = ORIENTED_EDGE ( 'NONE', *, *, #5645, .F. ) ;
#2587 = AXIS2_PLACEMENT_3D ( 'NONE', #7667, #4199, #14427 ) ;
#2588 = CARTESIAN_POINT ( 'NONE',  ( -5.248988766908546211, 2.532174945215636797, -4.566961984436638922 ) ) ;
#2589 = MECHANICAL_DESIGN_GEOMETRIC_PRESENTATION_REPRESENTATION (  '', ( #8435 ), #6081 ) ;
#2590 = DIRECTION ( 'NONE',  ( 1.000000000000000000, -2.551526159633733968E-19, -1.987661601597216239E-18 ) ) ;
#2591 = DIRECTION ( 'NONE',  ( 0.000000000000000000, 0.000000000000000000, 1.000000000000000000 ) ) ;
#2592 = DIRECTION ( 'NONE',  ( 1.000000000000000000, 0.000000000000000000, 0.000000000000000000 ) ) ;
#2593 = VECTOR ( 'NONE', #5356, 1000.000000000000000 ) ;
#2594 = ORIENTED_EDGE ( 'NONE', *, *, #4608, .F. ) ;
#2595 = DIRECTION ( 'NONE',  ( 0.000000000000000000, 0.000000000000000000, 1.000000000000000000 ) ) ;
#2596 = CARTESIAN_POINT ( 'NONE',  ( 108.6817075744280174, 109.5765550933605113, 1.102182119232617753E-14 ) ) ;
#2597 = CARTESIAN_POINT ( 'NONE',  ( 20.00000000000000355, 40.00000000000000711, -25.00000000000000000 ) ) ;
#2598 = ORIENTED_EDGE ( 'NONE', *, *, #13375, .T. ) ;
#2599 = CARTESIAN_POINT ( 'NONE',  ( 4.844561581013297591, -3.861881939214885762, -1.311024268447341656 ) ) ;
#2600 = VECTOR ( 'NONE', #13843, 1000.000000000000000 ) ;
#2601 = CARTESIAN_POINT ( 'NONE',  ( 5.085139881807313245, 4.657383176246348455, -0.06682429157517222329 ) ) ;
#2602 = CIRCLE ( 'NONE', #5843, 2.500000000000002220 ) ;
#2603 = VERTEX_POINT ( 'NONE', #13163 ) ;
#2604 = DIRECTION ( 'NONE',  ( 1.000000000000000000, 3.286707217423839940E-17, 2.273843122241288053E-18 ) ) ;
#2605 = ORIENTED_EDGE ( 'NONE', *, *, #12783, .T. ) ;
#2606 = EDGE_LOOP ( 'NONE', ( #14177, #5927, #335, #11394, #3892, #3979, #10224, #1426 ) ) ;
#2607 = DIRECTION ( 'NONE',  ( -1.000000000000000000, 0.000000000000000000, 0.000000000000000000 ) ) ;
#2608 = CARTESIAN_POINT ( 'NONE',  ( 0.000000000000000000, 0.000000000000000000, 13.31572692736082786 ) ) ;
#2609 = ORIENTED_EDGE ( 'NONE', *, *, #4181, .F. ) ;
#2610 = CARTESIAN_POINT ( 'NONE',  ( 0.3126073911696169993, 2.020725942163681399, -3.499999999999996003 ) ) ;
#2611 = ADVANCED_FACE ( 'NONE', ( #4378 ), #4237, .F. ) ;
#2612 = CARTESIAN_POINT ( 'NONE',  ( 19.99999999999999645, 57.00000000000000000, 25.00000000000000000 ) ) ;
#2613 = DIRECTION ( 'NONE',  ( 0.000000000000000000, -1.000000000000000000, 0.000000000000000000 ) ) ;
#2614 = PLANE ( 'NONE',  #11399 ) ;
#2615 = AXIS2_PLACEMENT_3D ( 'NONE', #4418, #12371, #7671 ) ;
#2616 = SURFACE_SIDE_STYLE ('',( #5960 ) ) ;
#2617 = LINE ( 'NONE', #1294, #3303 ) ;
#2618 = CARTESIAN_POINT ( 'NONE',  ( 0.3126073911696169993, 4.041451884327390331, 0.000000000000000000 ) ) ;
#2619 = CARTESIAN_POINT ( 'NONE',  ( 108.6817075744280174, -20.42344490663938572, 33.00000000000002842 ) ) ;
#2620 = CARTESIAN_POINT ( 'NONE',  ( 4.814824860968092917E-32, 4.618802153517016507, -3.204269196027521360 ) ) ;
#2621 = VERTEX_POINT ( 'NONE', #844 ) ;
#2622 = AXIS2_PLACEMENT_3D ( 'NONE', #2608, #10427, #13957 ) ;
#2623 = EDGE_CURVE ( 'NONE', #1594, #11164, #8747, .T. ) ;
#2624 = MECHANICAL_DESIGN_GEOMETRIC_PRESENTATION_REPRESENTATION (  '', ( #10328 ), #11983 ) ;
#2625 = VERTEX_POINT ( 'NONE', #2023 ) ;
#2626 = CIRCLE ( 'NONE', #10812, 2.100000000000000977 ) ;
#2627 = ORIENTED_EDGE ( 'NONE', *, *, #685, .T. ) ;
#2628 = LINE ( 'NONE', #9428, #14127 ) ;
#2629 = VERTEX_POINT ( 'NONE', #10734 ) ;
#2630 = ORIENTED_EDGE ( 'NONE', *, *, #8123, .T. ) ;
#2631 = CARTESIAN_POINT ( 'NONE',  ( 59.10586122665984732, -20.42344490663941414, -35.00000000000000000 ) ) ;
#2632 = EDGE_CURVE ( 'NONE', #6805, #8967, #3709, .T. ) ;
#2633 = LINE ( 'NONE', #13548, #9880 ) ;
#2634 = CARTESIAN_POINT ( 'NONE',  ( 88.22284556172391490, 29.57655509336062849, 33.00000000000002842 ) ) ;
#2635 = B_SPLINE_CURVE_WITH_KNOTS ( 'NONE', 3,
 ( #10342, #321, #12750, #4782, #8129, #8207 ),
 .UNSPECIFIED., .F., .F.,
 ( 4, 2, 4 ),
 ( 0.002365888236227976869, 0.003551327329835078477, 0.004736766423442180518 ),
 .UNSPECIFIED. ) ;
#2636 = CARTESIAN_POINT ( 'NONE',  ( 108.6817075744280174, 69.57655509336049704, 1.592040838891559450E-14 ) ) ;
#2637 = FACE_OUTER_BOUND ( 'NONE', #10692, .T. ) ;
#2638 = DIRECTION ( 'NONE',  ( 1.000000000000000000, 0.000000000000000000, 0.000000000000000000 ) ) ;
#2639 = CARTESIAN_POINT ( 'NONE',  ( 5.091953023115928900, 2.341213539480256234, 4.055100801747967054 ) ) ;
#2640 = DIRECTION ( 'NONE',  ( 0.000000000000000000, 0.000000000000000000, 1.000000000000000000 ) ) ;
#2641 = AXIS2_PLACEMENT_3D ( 'NONE', #3840, #11649, #1707 ) ;
#2642 = CONICAL_SURFACE ( 'NONE', #3578, 4.000000000000004441, 1.047197551196600296 ) ;
#2643 = PRODUCT ( 'hex flange nut gradea_iso_ISO - 4161 - M6 - N', 'hex flange nut gradea_iso_ISO - 4161 - M6 - N', '', ( #9658 ) ) ;
#2644 = LINE ( 'NONE', #13638, #12931 ) ;
#2645 = EDGE_LOOP ( 'NONE', ( #2594, #11262 ) ) ;
#2646 = EDGE_CURVE ( 'NONE', #435, #5824, #8675, .T. ) ;
#2647 = ORIENTED_EDGE ( 'NONE', *, *, #4064, .T. ) ;
#2648 = EDGE_LOOP ( 'NONE', ( #7129, #6996, #1399, #13359, #7830, #4340, #3185 ) ) ;
#2649 = ORIENTED_EDGE ( 'NONE', *, *, #11568, .F. ) ;
#2650 = VECTOR ( 'NONE', #13343, 1000.000000000000000 ) ;
#2651 = DIRECTION ( 'NONE',  ( 0.000000000000000000, 0.000000000000000000, -1.000000000000000000 ) ) ;
#2652 = PLANE ( 'NONE',  #13136 ) ;
#2653 = B_SPLINE_CURVE_WITH_KNOTS ( 'NONE', 3,
 ( #3181, #11137, #6444, #12097, #5504, #9972 ),
 .UNSPECIFIED., .F., .F.,
 ( 4, 2, 4 ),
 ( 0.000000000000000000, 0.002086519881787261485, 0.004173039763574522970 ),
 .UNSPECIFIED. ) ;
#2654 = PRESENTATION_STYLE_ASSIGNMENT (( #1476 ) ) ;
#2655 = ORIENTED_EDGE ( 'NONE', *, *, #2194, .F. ) ;
#2656 = DIRECTION ( 'NONE',  ( 0.000000000000000000, 0.000000000000000000, -1.000000000000000000 ) ) ;
#2657 = CARTESIAN_POINT ( 'NONE',  ( 5.084394237956035845, 2.335963250529156543, -4.046007034530243907 ) ) ;
#2658 = ORIENTED_EDGE ( 'NONE', *, *, #12379, .T. ) ;
#2659 = EDGE_CURVE ( 'NONE', #12223, #11750, #9069, .T. ) ;
#2660 = CARTESIAN_POINT ( 'NONE',  ( 32.60000000000000142, 29.99999999999999645, -34.50000000000000000 ) ) ;
#2661 = ORIENTED_EDGE ( 'NONE', *, *, #12092, .F. ) ;
#2662 = ADVANCED_FACE ( 'NONE', ( #14250 ), #9709, .T. ) ;
#2663 = VECTOR ( 'NONE', #10225, 1000.000000000000000 ) ;
#2664 = ORIENTED_EDGE ( 'NONE', *, *, #11015, .F. ) ;
#2665 = UNCERTAINTY_MEASURE_WITH_UNIT (LENGTH_MEASURE( 1.000000000000000082E-05 ), #2975, 'distance_accuracy_value', 'NONE');
#2666 = DIRECTION ( 'NONE',  ( -1.000000000000000000, 0.000000000000000000, 0.000000000000000000 ) ) ;
#2667 = CARTESIAN_POINT ( 'NONE',  ( 22.00000000000000000, 57.00000000000000000, 25.00000000000000000 ) ) ;
#2668 = ORIENTED_EDGE ( 'NONE', *, *, #9947, .T. ) ;
#2669 = CARTESIAN_POINT ( 'NONE',  ( 4.104070371397483541, -2.023683613428362005, -3.505122836902505146 ) ) ;
#2670 = CARTESIAN_POINT ( 'NONE',  ( 118.6817075744280601, 199.5765550933606107, 33.00000000000002842 ) ) ;
#2671 = CARTESIAN_POINT ( 'NONE',  ( 71.80728622811317052, -17.99808865627608512, -28.00000000000000000 ) ) ;
#2672 = DIRECTION ( 'NONE',  ( -1.000000000000000000, 0.000000000000000000, 0.000000000000000000 ) ) ;
#2673 = VERTEX_POINT ( 'NONE', #7491 ) ;
#2674 = CARTESIAN_POINT ( 'NONE',  ( 118.6817075744280174, -30.42344490663937506, 33.00000000000002842 ) ) ;
#2675 = VECTOR ( 'NONE', #3787, 1000.000000000000000 ) ;
#2676 = ORIENTED_EDGE ( 'NONE', *, *, #6472, .F. ) ;
#2677 = CARTESIAN_POINT ( 'NONE',  ( 7.500000000000029310, 29.99999999999999289, 8.000000000000007105 ) ) ;
#2678 = ORIENTED_EDGE ( 'NONE', *, *, #8571, .T. ) ;
#2679 = DIRECTION ( 'NONE',  ( 0.000000000000000000, 8.482162385747133845E-47, -1.000000000000000000 ) ) ;
#2680 = EDGE_CURVE ( 'NONE', #1178, #5665, #8815, .T. ) ;
#2681 = CARTESIAN_POINT ( 'NONE',  ( 22.00000000000000355, 27.00000000000000355, -25.00000000000000000 ) ) ;
#2682 = EDGE_LOOP ( 'NONE', ( #6005, #6143, #572, #4410, #10204 ) ) ;
#2683 = ADVANCED_FACE ( 'NONE', ( #13297 ), #788, .F. ) ;
#2684 = VERTEX_POINT ( 'NONE', #3272 ) ;
#2685 = CARTESIAN_POINT ( 'NONE',  ( 5.102759246810695259, 4.706121570500113371, -6.938893903907228378E-14 ) ) ;
#2686 = ORIENTED_EDGE ( 'NONE', *, *, #11415, .T. ) ;
#2687 = VERTEX_POINT ( 'NONE', #7714 ) ;
#2688 = CARTESIAN_POINT ( 'NONE',  ( 76.68170757442804586, -20.42344490663941414, -199.4258611313499330 ) ) ;
#2689 = CARTESIAN_POINT ( 'NONE',  ( 0.3572655899082288755, 4.618802153517023612, 1.387778780781445676E-14 ) ) ;
#2690 = ORIENTED_EDGE ( 'NONE', *, *, #11605, .T. ) ;
#2691 = ADVANCED_FACE ( 'NONE', ( #14116 ), #6465, .T. ) ;
#2692 = FACE_OUTER_BOUND ( 'NONE', #4554, .T. ) ;
#2693 = CARTESIAN_POINT ( 'NONE',  ( 56.75585977000769589, 23.28432498401347672, 25.00000000000000000 ) ) ;
#2694 = LINE ( 'NONE', #715, #5098 ) ;
#2695 = DIRECTION ( 'NONE',  ( -1.000000000000000000, 0.000000000000000000, 0.000000000000000000 ) ) ;
#2696 = ITEM_DEFINED_TRANSFORMATION ( 'NONE', 'NONE', #4093,  #11025 ) ;
#2697 = DIRECTION ( 'NONE',  ( 1.000000000000000000, 0.000000000000000000, 0.000000000000000000 ) ) ;
#2698 = CARTESIAN_POINT ( 'NONE',  ( -3.999999999999992006, 0.8576023918602521112, -3.133238574225018613 ) ) ;
#2699 = CARTESIAN_POINT ( 'NONE',  ( 68.68170757442801744, -83.66032599071898801, -117.0000000000000000 ) ) ;
#2700 = DIRECTION ( 'NONE',  ( -0.000000000000000000, -1.000000000000000000, 0.000000000000000000 ) ) ;
#2701 = EDGE_CURVE ( 'NONE', #11645, #2779, #7907, .T. ) ;
#2702 = EDGE_CURVE ( 'NONE', #12991, #7983, #6334, .T. ) ;
#2703 = VERTEX_POINT ( 'NONE', #5245 ) ;
#2704 = CARTESIAN_POINT ( 'NONE',  ( 76.68170757442801744, 144.5765550933605823, -199.4258611313499330 ) ) ;
#2705 = ORIENTED_EDGE ( 'NONE', *, *, #3724, .F. ) ;
#2706 = EDGE_CURVE ( 'NONE', #4722, #12253, #4867, .T. ) ;
#2707 = DIRECTION ( 'NONE',  ( -0.000000000000000000, 0.000000000000000000, 1.000000000000000000 ) ) ;
#2708 = CARTESIAN_POINT ( 'NONE',  ( -1.654252653721914434, -3.663718938583019558, -0.01223254789874345973 ) ) ;
#2709 = CARTESIAN_POINT ( 'NONE',  ( 0.000000000000000000, 0.000000000000000000, 0.000000000000000000 ) ) ;
#2710 = CONICAL_SURFACE ( 'NONE', #10879, 3.499999999999999112, 1.047197551196600296 ) ;
#2711 =( REPRESENTATION_RELATIONSHIP ('NONE','NONE', #10295, #852 ) REPRESENTATION_RELATIONSHIP_WITH_TRANSFORMATION ( #12284 )SHAPE_REPRESENTATION_RELATIONSHIP( ) );
#2712 = DIRECTION ( 'NONE',  ( 0.000000000000000000, 0.000000000000000000, 1.000000000000000000 ) ) ;
#2713 = CARTESIAN_POINT ( 'NONE',  ( 5.102759246810640192, -2.353060785250063347, -4.075620833351001338 ) ) ;
#2714 = CARTESIAN_POINT ( 'NONE',  ( -3.822382184081044798, 10.25936179483149324, 0.000000000000000000 ) ) ;
#2715 = DIRECTION ( 'NONE',  ( 1.000000000000000000, 0.000000000000000000, 0.000000000000000000 ) ) ;
#2716 = EDGE_CURVE ( 'NONE', #2174, #4711, #11982, .T. ) ;
#2717 = CARTESIAN_POINT ( 'NONE',  ( -4.197393957002300446, -7.772664289393031077E-14, -3.203767560748911780 ) ) ;
#2718 = ADVANCED_FACE ( 'NONE', ( #9771 ), #10939, .T. ) ;
#2719 = LINE ( 'NONE', #13632, #9855 ) ;
#2720 = CARTESIAN_POINT ( 'NONE',  ( 31.38313257588138683, 143.6985259526510390, 28.00000000000000000 ) ) ;
#2721 = ADVANCED_FACE ( 'NONE', ( #9165 ), #11227, .T. ) ;
#2722 = ORIENTED_EDGE ( 'NONE', *, *, #12323, .F. ) ;
#2723 = EDGE_CURVE ( 'NONE', #11645, #12380, #9019, .T. ) ;
#2724 = VERTEX_POINT ( 'NONE', #6899 ) ;
#2725 = VERTEX_POINT ( 'NONE', #4588 ) ;
#2726 = DIRECTION ( 'NONE',  ( -0.9701425001453318764, -0.2425356250363329969, 0.000000000000000000 ) ) ;
#2727 = FACE_OUTER_BOUND ( 'NONE', #642, .T. ) ;
#2728 = FILL_AREA_STYLE ('',( #12662 ) ) ;
#2729 = EDGE_CURVE ( 'NONE', #3826, #3362, #6267, .T. ) ;
#2730 = ORIENTED_EDGE ( 'NONE', *, *, #8142, .T. ) ;
#2731 = ORIENTED_EDGE ( 'NONE', *, *, #9196, .T. ) ;
#2732 = PLANE ( 'NONE',  #6481 ) ;
#2733 = LINE ( 'NONE', #6069, #14313 ) ;
#2734 = CIRCLE ( 'NONE', #10898, 3.299999999999983391 ) ;
#2735 = ORIENTED_EDGE ( 'NONE', *, *, #9535, .T. ) ;
#2736 = FACE_BOUND ( 'NONE', #13542, .T. ) ;
#2737 = LINE ( 'NONE', #4849, #1242 ) ;
#2738 = DIRECTION ( 'NONE',  ( 0.000000000000000000, 0.000000000000000000, -1.000000000000000000 ) ) ;
#2739 = VERTEX_POINT ( 'NONE', #6688 ) ;
#2740 = DIRECTION ( 'NONE',  ( 0.000000000000000000, -0.000000000000000000, 1.000000000000000000 ) ) ;
#2741 = FACE_BOUND ( 'NONE', #3207, .T. ) ;
#2742 = SURFACE_SIDE_STYLE ('',( #8211 ) ) ;
#2743 = ORIENTED_EDGE ( 'NONE', *, *, #9653, .T. ) ;
#2744 = CYLINDRICAL_SURFACE ( 'NONE', #13264, 2.499999999999999112 ) ;
#2745 = EDGE_CURVE ( 'NONE', #2216, #1356, #3906, .T. ) ;
#2746 = CARTESIAN_POINT ( 'NONE',  ( 92.68170757442806007, 124.5765550933605965, 25.00000000000000000 ) ) ;
#2747 = AXIS2_PLACEMENT_3D ( 'NONE', #5724, #10200, #186 ) ;
#2748 = VERTEX_POINT ( 'NONE', #5786 ) ;
#2749 = SURFACE_STYLE_FILL_AREA ( #6088 ) ;
#2750 = VECTOR ( 'NONE', #2540, 1000.000000000000000 ) ;
#2751 = ORIENTED_EDGE ( 'NONE', *, *, #1688, .F. ) ;
#2752 = LINE ( 'NONE', #2829, #5547 ) ;
#2753 = CARTESIAN_POINT ( 'NONE',  ( 4.235887314095731604, 2.417314327725962997, -3.451162025751971729 ) ) ;
#2754 = EDGE_LOOP ( 'NONE', ( #12609, #12486, #4903, #9949, #10444, #785, #12523, #13410, #5775, #4321, #6309, #3499, #649, #13958, #10226, #1836, #226, #164, #12811, #12934, #121, #8467, #8808, #8615, #11419, #2831, #2476, #7743, #10745, #7634 ) ) ;
#2755 = DIRECTION ( 'NONE',  ( 1.000000000000000000, 0.000000000000000000, 0.000000000000000000 ) ) ;
#2756 = FACE_BOUND ( 'NONE', #2206, .T. ) ;
#2757 = AXIS2_PLACEMENT_3D ( 'NONE', #4083, #13073, #6319 ) ;
#2758 = CARTESIAN_POINT ( 'NONE',  ( 5.099999999999993427, 3.481583491540829278E-16, -5.200000000000001066 ) ) ;
#2759 = ORIENTED_EDGE ( 'NONE', *, *, #6035, .T. ) ;
#2760 = VECTOR ( 'NONE', #6987, 1000.000000000000000 ) ;
#2761 = ORIENTED_EDGE ( 'NONE', *, *, #3247, .F. ) ;
#2762 = FACE_OUTER_BOUND ( 'NONE', #590, .T. ) ;
#2763 = CARTESIAN_POINT ( 'NONE',  ( 0.1391502195351453364, 4.241015250120821811, -0.6543461111163241251 ) ) ;
#2764 = ORIENTED_EDGE ( 'NONE', *, *, #3771, .F. ) ;
#2765 = PLANE ( 'NONE',  #4916 ) ;
#2766 = CARTESIAN_POINT ( 'NONE',  ( 0.1586754815284855125, -2.687817229851451994, 3.344563996438223885 ) ) ;
#2767 = DIRECTION ( 'NONE',  ( 0.000000000000000000, 0.000000000000000000, -1.000000000000000000 ) ) ;
#2768 = EDGE_CURVE ( 'NONE', #13171, #14126, #7895, .T. ) ;
#2769 = CARTESIAN_POINT ( 'NONE',  ( 54.33050351964436686, 32.98574998546678927, 25.00000000000000000 ) ) ;
#2770 = EDGE_CURVE ( 'NONE', #10977, #12581, #2379, .T. ) ;
#2771 = CARTESIAN_POINT ( 'NONE',  ( 105.6817075744280174, 109.5765550933605113, -3.299999999999986500 ) ) ;
#2772 = CARTESIAN_POINT ( 'NONE',  ( 56.75585977000769589, 23.28432498401347672, 25.00000000000000000 ) ) ;
#2773 = AXIS2_PLACEMENT_3D ( 'NONE', #952, #4494, #9812 ) ;
#2774 = CARTESIAN_POINT ( 'NONE',  ( 0.000000000000000000, 0.000000000000000000, -106.9999999999999858 ) ) ;
#2775 = CARTESIAN_POINT ( 'NONE',  ( 4.104070371397483541, 2.023683613428362005, -3.505122836902505146 ) ) ;
#2776 = VECTOR ( 'NONE', #10811, 1000.000000000000000 ) ;
#2777 = FACE_OUTER_BOUND ( 'NONE', #11779, .T. ) ;
#2778 = AXIS2_PLACEMENT_3D ( 'NONE', #3914, #4929, #9316 ) ;
#2779 = VERTEX_POINT ( 'NONE', #5522 ) ;
#2780 = ORIENTED_EDGE ( 'NONE', *, *, #12032, .F. ) ;
#2781 = CARTESIAN_POINT ( 'NONE',  ( 4.000000000000003553, 2.309401076758501592, -3.133295621305376422 ) ) ;
#2782 = VERTEX_POINT ( 'NONE', #1206 ) ;
#2783 = CIRCLE ( 'NONE', #196, 4.000000000000004441 ) ;
#2784 = EDGE_LOOP ( 'NONE', ( #6969, #8666, #10622, #8524, #1694, #54, #9238 ) ) ;
#2785 = CIRCLE ( 'NONE', #8372, 5.200000000000001066 ) ;
#2786 = DIRECTION ( 'NONE',  ( 0.000000000000000000, 0.000000000000000000, 1.000000000000000000 ) ) ;
#2787 = CARTESIAN_POINT ( 'NONE',  ( 22.00000000000000355, 30.00000000000000711, -25.00000000000000000 ) ) ;
#2788 = DIRECTION ( 'NONE',  ( 0.000000000000000000, 0.000000000000000000, 1.000000000000000000 ) ) ;
#2789 = AXIS2_PLACEMENT_3D ( 'NONE', #8599, #3200, #3065 ) ;
#2790 = DIRECTION ( 'NONE',  ( 0.5000000000000022204, -0.8660254037844373753, -8.404057939144332757E-32 ) ) ;
#2791 = CARTESIAN_POINT ( 'NONE',  ( 8.000000000000000000, 40.49999999999999289, 8.000000000000007105 ) ) ;
#2792 = DIRECTION ( 'NONE',  ( -1.276920294826117846E-16, 0.000000000000000000, -1.000000000000000000 ) ) ;
#2793 = CARTESIAN_POINT ( 'NONE',  ( 99.68170757442806007, 109.5765550933604686, 1.102106265879292722E-14 ) ) ;
#2794 = DIRECTION ( 'NONE',  ( 0.000000000000000000, 0.000000000000000000, -1.000000000000000000 ) ) ;
#2795 = CARTESIAN_POINT ( 'NONE',  ( -68.68170757442808849, 39.57655509336051836, -117.0000000000000000 ) ) ;
#2796 = CARTESIAN_POINT ( 'NONE',  ( -3.999999999999996447, -2.309401076758511806, -0.5000000000000004441 ) ) ;
#2797 = ORIENTED_EDGE ( 'NONE', *, *, #7441, .F. ) ;
#2798 = ORIENTED_EDGE ( 'NONE', *, *, #3771, .T. ) ;
#2799 = EDGE_CURVE ( 'NONE', #12483, #8354, #12334, .T. ) ;
#2800 = FACE_OUTER_BOUND ( 'NONE', #8243, .T. ) ;
#2801 = DIRECTION ( 'NONE',  ( 0.000000000000000000, 0.000000000000000000, 1.000000000000000000 ) ) ;
#2802 = CIRCLE ( 'NONE', #9799, 2.750000000000003553 ) ;
#2803 =( LENGTH_UNIT ( ) NAMED_UNIT ( * ) SI_UNIT ( .MILLI., .METRE. ) );
#2804 = ADVANCED_FACE ( 'NONE', ( #9993 ), #6736, .T. ) ;
#2805 = EDGE_CURVE ( 'NONE', #12241, #7901, #10264, .T. ) ;
#2806 = VERTEX_POINT ( 'NONE', #1277 ) ;
#2807 = EDGE_LOOP ( 'NONE', ( #8996, #8842, #8731, #3228, #7372, #7411 ) ) ;
#2808 = LINE ( 'NONE', #11646, #7887 ) ;
#2809 = CARTESIAN_POINT ( 'NONE',  ( 4.000000000000003553, 0.9868501483902586413, -0.09357334158579964922 ) ) ;
#2810 = ORIENTED_EDGE ( 'NONE', *, *, #7459, .F. ) ;
#2811 = CARTESIAN_POINT ( 'NONE',  ( 28.00000000000000355, 29.99999999999999645, 0.000000000000000000 ) ) ;
#2812 = B_SPLINE_CURVE_WITH_KNOTS ( 'NONE', 3,
 ( #11082, #1196, #7919, #6889, #6679, #12324 ),
 .UNSPECIFIED., .F., .F.,
 ( 4, 2, 4 ),
 ( 0.006655250997664750867, 0.007825277639709792357, 0.008995304281754833847 ),
 .UNSPECIFIED. ) ;
#2813 = AXIS2_PLACEMENT_3D ( 'NONE', #7440, #925, #13239 ) ;
#2814 = ADVANCED_FACE ( 'NONE', ( #12474 ), #4454, .F. ) ;
#2815 = UNCERTAINTY_MEASURE_WITH_UNIT (LENGTH_MEASURE( 1.000000000000000082E-05 ), #12457, 'distance_accuracy_value', 'NONE');
#2816 = CARTESIAN_POINT ( 'NONE',  ( 0.3572655899081733644, 2.309401076758504701, -3.999999999999989786 ) ) ;
#2817 = CARTESIAN_POINT ( 'NONE',  ( 62.10586122665987574, -20.42344490663940704, -28.00000000000000000 ) ) ;
#2818 = CARTESIAN_POINT ( 'NONE',  ( 0.03363697881402510914, -0.7786124122131015124, 4.000000000000004441 ) ) ;
#2819 = ORIENTED_EDGE ( 'NONE', *, *, #7762, .T. ) ;
#2820 = CARTESIAN_POINT ( 'NONE',  ( 4.132952817037849336, 4.063368025374519910, -6.938893903907228378E-15 ) ) ;
#2821 = DIRECTION ( 'NONE',  ( -0.2425356250363328581, 0.9701425001453318764, -0.000000000000000000 ) ) ;
#2822 = ADVANCED_FACE ( 'NONE', ( #10059 ), #3349, .F. ) ;
#2823 = ORIENTED_EDGE ( 'NONE', *, *, #10457, .F. ) ;
#2824 = CARTESIAN_POINT ( 'NONE',  ( 59.10586122665984732, -20.42344490663941414, 35.00000000000000000 ) ) ;
#2825 = CARTESIAN_POINT ( 'NONE',  ( -5.000000000000001776, -2.886751345948152192, -0.5999999999999894307 ) ) ;
#2826 = ORIENTED_EDGE ( 'NONE', *, *, #3829, .F. ) ;
#2827 = CARTESIAN_POINT ( 'NONE',  ( 60.00000000000000000, -6.123233995736768255E-16, -23.00000000000000000 ) ) ;
#2828 = CIRCLE ( 'NONE', #3522, 3.299999999999983391 ) ;
#2829 = CARTESIAN_POINT ( 'NONE',  ( -129.3408537872145132, 189.5765550933606107, -70.00000000000000000 ) ) ;
#2830 = FACE_OUTER_BOUND ( 'NONE', #3497, .T. ) ;
#2831 = ORIENTED_EDGE ( 'NONE', *, *, #4707, .F. ) ;
#2832 = DIRECTION ( 'NONE',  ( 0.000000000000000000, 0.000000000000000000, 1.000000000000000000 ) ) ;
#2833 = FACE_BOUND ( 'NONE', #10951, .T. ) ;
#2834 = CARTESIAN_POINT ( 'NONE',  ( -2.500000000000002220, -4.163336342344338999E-16, -4.674599999999973221 ) ) ;
#2835 = EDGE_LOOP ( 'NONE', ( #7365, #10921, #3475, #8407 ) ) ;
#2836 = EDGE_CURVE ( 'NONE', #3862, #4403, #180, .T. ) ;
#2837 = VECTOR ( 'NONE', #366, 1000.000000000000000 ) ;
#2838 = VERTEX_POINT ( 'NONE', #3561 ) ;
#2839 = CARTESIAN_POINT ( 'NONE',  ( 76.68170757442798902, 124.5765550933606249, 25.00000000000000000 ) ) ;
#2840 = DIRECTION ( 'NONE',  ( 0.000000000000000000, 0.000000000000000000, -1.000000000000000000 ) ) ;
#2841 = VERTEX_POINT ( 'NONE', #9093 ) ;
#2842 = CIRCLE ( 'NONE', #10995, 2.500000000000002220 ) ;
#2843 = CARTESIAN_POINT ( 'NONE',  ( 4.180231891692620216, 4.134807952925580565, 0.02076457676760649559 ) ) ;
#2844 = DIRECTION ( 'NONE',  ( 1.000000000000000000, 0.000000000000000000, 0.000000000000000000 ) ) ;
#2845 = CARTESIAN_POINT ( 'NONE',  ( 54.40514726928103784, 42.68717498692012668, -25.00000000000000000 ) ) ;
#2846 = CARTESIAN_POINT ( 'NONE',  ( 60.00000000000000000, -6.123233995736768255E-16, -25.00000000000000000 ) ) ;
#2847 = VERTEX_POINT ( 'NONE', #2242 ) ;
#2848 = B_SPLINE_CURVE_WITH_KNOTS ( 'NONE', 3,
 ( #4125, #6142, #10759, #12978, #7385, #9663, #13992, #1608, #3891, #6286 ),
 .UNSPECIFIED., .F., .F.,
 ( 4, 2, 2, 2, 4 ),
 ( 1.451678239244173839E-19, 0.001528561485809837566, 0.003057122971619674699, 0.004585684457429510530, 0.006114245943239346795 ),
 .UNSPECIFIED. ) ;
#2849 = CARTESIAN_POINT ( 'NONE',  ( 5.733169058567799681, -6.938893903907228378E-15, 0.000000000000000000 ) ) ;
#2850 = CARTESIAN_POINT ( 'NONE',  ( 4.755015822784813828, 0.000000000000000000, 0.000000000000000000 ) ) ;
#2851 = DIRECTION ( 'NONE',  ( 0.000000000000000000, 0.000000000000000000, -1.000000000000000000 ) ) ;
#2852 = STYLED_ITEM ( 'NONE', ( #9618 ), #11938 ) ;
#2853 = DIRECTION ( 'NONE',  ( 0.000000000000000000, 0.000000000000000000, -1.000000000000000000 ) ) ;
#2854 = VECTOR ( 'NONE', #5767, 1000.000000000000000 ) ;
#2855 = EDGE_CURVE ( 'NONE', #13646, #10382, #1135, .T. ) ;
#2856 = PRODUCT_RELATED_PRODUCT_CATEGORY ( 'part', '', ( #3579 ) ) ;
#2857 = ADVANCED_FACE ( 'NONE', ( #4523 ), #1034, .F. ) ;
#2858 = VERTEX_POINT ( 'NONE', #631 ) ;
#2859 = CARTESIAN_POINT ( 'NONE',  ( 25.90000000000000213, 29.99999999999999645, -25.00000000000000000 ) ) ;
#2860 = ORIENTED_EDGE ( 'NONE', *, *, #293, .T. ) ;
#2861 = ORIENTED_EDGE ( 'NONE', *, *, #7993, .T. ) ;
#2862 = LINE ( 'NONE', #12874, #11439 ) ;
#2863 = TOROIDAL_SURFACE ( 'NONE', #4714, 6.250000000000000000, 0.5499999999999992673 ) ;
#2864 = CARTESIAN_POINT ( 'NONE',  ( -88.22284556172398595, 39.57655509336048283, -106.9999999999999858 ) ) ;
#2865 = CARTESIAN_POINT ( 'NONE',  ( 18.12748877629582367, 43.82334295289049919, 8.000000000000007105 ) ) ;
#2866 = DIRECTION ( 'NONE',  ( 1.000000000000000000, 0.000000000000000000, 0.000000000000000000 ) ) ;
#2867 = DIRECTION ( 'NONE',  ( 0.000000000000000000, 0.000000000000000000, -1.000000000000000000 ) ) ;
#2868 = SHAPE_DEFINITION_REPRESENTATION ( #11381, #7856 ) ;
#2869 = CARTESIAN_POINT ( 'NONE',  ( 3.510273485745313948, 2.827716139362655756, -3.310536846335870642 ) ) ;
#2870 = CARTESIAN_POINT ( 'NONE',  ( 3.961551342853563806, -3.742715940867795688, 0.5174258321190287058 ) ) ;
#2871 = ORIENTED_EDGE ( 'NONE', *, *, #10301, .T. ) ;
#2872 = CIRCLE ( 'NONE', #7287, 3.299999999999983391 ) ;
#2873 = MECHANICAL_DESIGN_GEOMETRIC_PRESENTATION_REPRESENTATION (  '', ( #5426 ), #12446 ) ;
#2874 = AXIS2_PLACEMENT_3D ( 'NONE', #1495, #4856, #1794 ) ;
#2875 = CARTESIAN_POINT ( 'NONE',  ( 0.3572655899080068309, -2.309401076758678339, -4.000000000000031086 ) ) ;
#2876 = ADVANCED_FACE ( 'NONE', ( #8284 ), #10414, .F. ) ;
#2877 = ORIENTED_EDGE ( 'NONE', *, *, #11196, .F. ) ;
#2878 = ORIENTED_EDGE ( 'NONE', *, *, #8871, .T. ) ;
#2879 = DIRECTION ( 'NONE',  ( -1.734723475976770502E-18, 4.440892098500621231E-16, 1.000000000000000000 ) ) ;
#2880 = CARTESIAN_POINT ( 'NONE',  ( 0.03027795055833587892, 0.6888063905328651870, 3.499999999999996891 ) ) ;
#2881 =( GEOMETRIC_REPRESENTATION_CONTEXT ( 3 ) GLOBAL_UNCERTAINTY_ASSIGNED_CONTEXT ( ( #13058 ) ) GLOBAL_UNIT_ASSIGNED_CONTEXT ( ( #10642, #12755, #3849 ) ) REPRESENTATION_CONTEXT ( 'NONE', 'WORKASPACE' ) );
#2882 = CIRCLE ( 'NONE', #991, 3.200000000000000622 ) ;
#2883 = AXIS2_PLACEMENT_3D ( 'NONE', #11718, #12079, #8988 ) ;
#2884 = ORIENTED_EDGE ( 'NONE', *, *, #11455, .T. ) ;
#2885 = B_SPLINE_CURVE_WITH_KNOTS ( 'NONE', 3,
 ( #6282, #12972, #8257, #12884, #10755, #2869, #6354, #9440 ),
 .UNSPECIFIED., .F., .F.,
 ( 4, 2, 2, 4 ),
 ( 5.712950814681226391E-18, 0.002450665683189820563, 0.003675998524784728026, 0.004901331366379636789 ),
 .UNSPECIFIED. ) ;
#2886 = EDGE_LOOP ( 'NONE', ( #9404, #12582, #13083, #11838 ) ) ;
#2887 = CARTESIAN_POINT ( 'NONE',  ( 4.319324222800735136, -3.279739689145003467, -4.138711833384554950 ) ) ;
#2888 = CARTESIAN_POINT ( 'NONE',  ( -0.8441225671336188840, -5.568793373799661772, -4.476900509771287062 ) ) ;
#2889 = ORIENTED_EDGE ( 'NONE', *, *, #12977, .F. ) ;
#2890 = APPLICATION_CONTEXT ( 'automotive_design' ) ;
#2891 = DIRECTION ( 'NONE',  ( 0.000000000000000000, -1.000000000000000000, 0.000000000000000000 ) ) ;
#2892 = VECTOR ( 'NONE', #6643, 1000.000000000000114 ) ;
#2893 = EDGE_CURVE ( 'NONE', #10783, #14055, #2303, .T. ) ;
#2894 = ORIENTED_EDGE ( 'NONE', *, *, #12073, .F. ) ;
#2895 = CARTESIAN_POINT ( 'NONE',  ( 1.560000000000005826, -0.8660254037844428154, -1.500000000000001332 ) ) ;
#2896 = FACE_OUTER_BOUND ( 'NONE', #5590, .T. ) ;
#2897 = CARTESIAN_POINT ( 'NONE',  ( 0.000000000000000000, 0.000000000000000000, 0.000000000000000000 ) ) ;
#2898 = VERTEX_POINT ( 'NONE', #11435 ) ;
#2899 = DIRECTION ( 'NONE',  ( 0.3420201433256618850, 5.322992421552529242E-16, 0.9396926207859108704 ) ) ;
#2900 = FACE_OUTER_BOUND ( 'NONE', #11574, .T. ) ;
#2901 = ORIENTED_EDGE ( 'NONE', *, *, #4793, .F. ) ;
#2902 = DIRECTION ( 'NONE',  ( -0.2425356250363330524, 0.9701425001453318764, 0.000000000000000000 ) ) ;
#2903 = DIRECTION ( 'NONE',  ( 1.000000000000000000, 0.000000000000000000, 0.000000000000000000 ) ) ;
#2904 = VECTOR ( 'NONE', #4860, 1000.000000000000000 ) ;
#2905 = ORIENTED_EDGE ( 'NONE', *, *, #9218, .F. ) ;
#2906 = CARTESIAN_POINT ( 'NONE',  ( 49.40514726928103073, 42.68717498692012668, 25.00000000000000000 ) ) ;
#2907 = CARTESIAN_POINT ( 'NONE',  ( 20.00000000000000000, -5.510910596163090344E-15, -25.00000000000000000 ) ) ;
#2908 = EDGE_CURVE ( 'NONE', #313, #5595, #8361, .T. ) ;
#2909 = CARTESIAN_POINT ( 'NONE',  ( 0.5276476219768478915, -4.314164656931422925, -3.020318136128777642 ) ) ;
#2910 = AXIS2_PLACEMENT_3D ( 'NONE', #10884, #13237, #10001 ) ;
#2911 = EDGE_LOOP ( 'NONE', ( #1875, #5174, #1539, #8169, #12998, #8548, #4295, #10199, #7142, #14194, #2469, #11280, #6522, #3009, #10776, #6460, #9470, #2889, #1950, #8452, #1981, #14109, #488, #9956, #9578, #6218, #9252, #2743, #11084, #4109 ) ) ;
#2912 = FACE_OUTER_BOUND ( 'NONE', #9549, .T. ) ;
#2913 = FACE_BOUND ( 'NONE', #8983, .T. ) ;
#2914 = EDGE_CURVE ( 'NONE', #12288, #10509, #3949, .T. ) ;
#2915 = PRODUCT_DEFINITION_FORMATION_WITH_SPECIFIED_SOURCE ( 'ANY', '', #3579, .NOT_KNOWN. ) ;
#2916 = CARTESIAN_POINT ( 'NONE',  ( 0.000000000000000000, 0.000000000000000000, 1.599999999999990319 ) ) ;
#2917 = ORIENTED_EDGE ( 'NONE', *, *, #9650, .F. ) ;
#2918 = VERTEX_POINT ( 'NONE', #6008 ) ;
#2919 = CARTESIAN_POINT ( 'NONE',  ( 2.949999999999994404, 0.000000000000000000, 0.000000000000000000 ) ) ;
#2920 = CARTESIAN_POINT ( 'NONE',  ( 20.00000000000000355, 17.00000000000000000, -25.00000000000000000 ) ) ;
#2921 = ORIENTED_EDGE ( 'NONE', *, *, #9960, .T. ) ;
#2922 = DIRECTION ( 'NONE',  ( -1.000000000000000000, -0.000000000000000000, -0.000000000000000000 ) ) ;
#2923 = CIRCLE ( 'NONE', #10839, 5.000000000000000888 ) ;
#2924 = CARTESIAN_POINT ( 'NONE',  ( 2.540000000000002700, 4.229949723821848943E-16, 1.599999999999990319 ) ) ;
#2925 = EDGE_LOOP ( 'NONE', ( #10674, #14163, #9249, #8632, #13072, #942, #12028, #2103 ) ) ;
#2926 = EDGE_CURVE ( 'NONE', #8962, #3669, #9391, .T. ) ;
#2927 = PRESENTATION_STYLE_ASSIGNMENT (( #10808 ) ) ;
#2928 = CARTESIAN_POINT ( 'NONE',  ( 4.180231680468786237, -2.085385483809543583, 3.570466434508598574 ) ) ;
#2929 = ORIENTED_EDGE ( 'NONE', *, *, #10810, .T. ) ;
#2930 = FACE_OUTER_BOUND ( 'NONE', #10865, .T. ) ;
#2931 = PLANE ( 'NONE',  #7167 ) ;
#2932 = EDGE_CURVE ( 'NONE', #6869, #11164, #12087, .T. ) ;
#2933 = PLANE ( 'NONE',  #9775 ) ;
#2934 = SHAPE_REPRESENTATION ( 'hex flange bolt small_iso_ISO 4162 - M5 x 25 x 16-N', ( #11025 ), #10318 ) ;
#2935 = ORIENTED_EDGE ( 'NONE', *, *, #5284, .F. ) ;
#2936 = DIRECTION ( 'NONE',  ( -1.000000000000000000, 0.000000000000000000, 0.000000000000000000 ) ) ;
#2937 = ORIENTED_EDGE ( 'NONE', *, *, #8949, .F. ) ;
#2938 = ORIENTED_EDGE ( 'NONE', *, *, #3583, .F. ) ;
#2939 = DIRECTION ( 'NONE',  ( 0.000000000000000000, 0.000000000000000000, -1.000000000000000000 ) ) ;
#2940 = DIRECTION ( 'NONE',  ( -0.000000000000000000, -1.000000000000000000, -0.000000000000000000 ) ) ;
#2941 = CARTESIAN_POINT ( 'NONE',  ( 1.305984381679704098, 48.39647413643795204, 0.2102513847387766921 ) ) ;
#2942 = CARTESIAN_POINT ( 'NONE',  ( 28.00000000000000355, 29.99999999999999645, 6.999999999999992006 ) ) ;
#2943 = DIRECTION ( 'NONE',  ( -0.9701425001453318764, -0.2425356250363329969, 0.000000000000000000 ) ) ;
#2944 = APPLICATION_PROTOCOL_DEFINITION ( 'draft international standard', 'automotive_design', 1998, #5833 ) ;
#2945 = FACE_BOUND ( 'NONE', #7169, .T. ) ;
#2946 = ADVANCED_FACE ( 'NONE', ( #12839 ), #2744, .T. ) ;
#2947 = CARTESIAN_POINT ( 'NONE',  ( 28.00000000000000355, 29.99999999999999645, -34.50000000000000000 ) ) ;
#2948 = DIRECTION ( 'NONE',  ( 1.000000000000000000, 0.000000000000000000, 0.000000000000000000 ) ) ;
#2949 = VERTEX_POINT ( 'NONE', #10346 ) ;
#2950 = ORIENTED_EDGE ( 'NONE', *, *, #11821, .F. ) ;
#2951 = ORIENTED_EDGE ( 'NONE', *, *, #2973, .F. ) ;
#2952 = CARTESIAN_POINT ( 'NONE',  ( 59.10586122665984732, -20.42344490663941414, -23.00000000000000000 ) ) ;
#2953 = CARTESIAN_POINT ( 'NONE',  ( 2.999999999999986233, -3.266600723550367725E-47, 5.421010862427522170E-17 ) ) ;
#2954 = ADVANCED_FACE ( 'NONE', ( #13942 ), #8360, .F. ) ;
#2955 = ORIENTED_EDGE ( 'NONE', *, *, #13772, .T. ) ;
#2956 = ADVANCED_FACE ( 'NONE', ( #6170 ), #14023, .F. ) ;
#2957 = CARTESIAN_POINT ( 'NONE',  ( 0.6806757771989077055, -5.380514348699644955, -4.138711833382306082 ) ) ;
#2958 = VECTOR ( 'NONE', #3985, 999.9999999999998863 ) ;
#2959 = CARTESIAN_POINT ( 'NONE',  ( 0.000000000000000000, 0.000000000000000000, 0.000000000000000000 ) ) ;
#2960 = ORIENTED_EDGE ( 'NONE', *, *, #7391, .T. ) ;
#2961 = LINE ( 'NONE', #10633, #4986 ) ;
#2962 = EDGE_LOOP ( 'NONE', ( #5208, #9213, #12484, #4801 ) ) ;
#2963 = UNCERTAINTY_MEASURE_WITH_UNIT (LENGTH_MEASURE( 1.000000000000000082E-05 ), #1746, 'distance_accuracy_value', 'NONE');
#2964 = DIRECTION ( 'NONE',  ( 0.000000000000000000, 0.000000000000000000, 1.000000000000000000 ) ) ;
#2965 = FACE_OUTER_BOUND ( 'NONE', #7500, .T. ) ;
#2966 = DIRECTION ( 'NONE',  ( 0.000000000000000000, -1.000000000000000000, 0.000000000000000000 ) ) ;
#2967 = EDGE_LOOP ( 'NONE', ( #456, #7975, #11692, #11861 ) ) ;
#2968 = CARTESIAN_POINT ( 'NONE',  ( 4.114405500665252013, 4.051151509359440794, -1.387744507531641370E-14 ) ) ;
#2969 = PLANE ( 'NONE',  #1075 ) ;
#2970 = EDGE_LOOP ( 'NONE', ( #8126, #1472, #6691 ) ) ;
#2971 = LINE ( 'NONE', #6388, #288 ) ;
#2972 = ORIENTED_EDGE ( 'NONE', *, *, #3550, .F. ) ;
#2973 = EDGE_CURVE ( 'NONE', #5297, #4637, #12601, .T. ) ;
#2974 = ADVANCED_BREP_SHAPE_REPRESENTATION ( '', ( #1997, #11025 ), #10318 ) ;
#2975 =( LENGTH_UNIT ( ) NAMED_UNIT ( * ) SI_UNIT ( .MILLI., .METRE. ) );
#2976 = ADVANCED_FACE ( 'NONE', ( #1494 ), #7111, .F. ) ;
#2977 = ORIENTED_EDGE ( 'NONE', *, *, #3326, .T. ) ;
#2978 = LINE ( 'NONE', #7347, #9045 ) ;
#2979 = DIRECTION ( 'NONE',  ( 0.000000000000000000, 0.000000000000000000, -1.000000000000000000 ) ) ;
#2980 = ORIENTED_EDGE ( 'NONE', *, *, #10911, .T. ) ;
#2981 = DIRECTION ( 'NONE',  ( 1.000000000000000000, 1.224646799147353454E-16, -0.000000000000000000 ) ) ;
#2982 = EDGE_CURVE ( 'NONE', #2838, #8043, #2132, .T. ) ;
#2983 = CARTESIAN_POINT ( 'NONE',  ( 20.00000000000000355, 30.00000000000000711, 25.00000000000000000 ) ) ;
#2984 = ORIENTED_EDGE ( 'NONE', *, *, #1152, .F. ) ;
#2985 = VERTEX_POINT ( 'NONE', #4346 ) ;
#2986 = VECTOR ( 'NONE', #2286, 1000.000000000000000 ) ;
#2987 = CARTESIAN_POINT ( 'NONE',  ( 3.951447005078477126, -1.347150628109121007, -3.500000000000011546 ) ) ;
#2988 = CARTESIAN_POINT ( 'NONE',  ( -3.012791009409888865, 47.91354231080889292, 6.643648411893776640 ) ) ;
#2989 = ADVANCED_FACE ( 'NONE', ( #88 ), #2523, .F. ) ;
#2990 = ORIENTED_EDGE ( 'NONE', *, *, #1500, .F. ) ;
#2991 = CARTESIAN_POINT ( 'NONE',  ( 4.175813232069169878, -4.122719923832743660, -6.938893903907228378E-15 ) ) ;
#2992 = DIRECTION ( 'NONE',  ( 1.000000000000000000, 3.916739600140467622E-15, 0.000000000000000000 ) ) ;
#2993 = FILL_AREA_STYLE ('',( #6260 ) ) ;
#2994 = CARTESIAN_POINT ( 'NONE',  ( 20.00000000000000355, 17.00000000000000000, -25.00000000000000000 ) ) ;
#2995 = VERTEX_POINT ( 'NONE', #13417 ) ;
#2996 = DIRECTION ( 'NONE',  ( 1.000000000000000000, 0.000000000000000000, 0.000000000000000000 ) ) ;
#2997 = ADVANCED_FACE ( 'NONE', ( #6579 ), #9808, .T. ) ;
#2998 = EDGE_CURVE ( 'NONE', #1264, #7901, #10715, .T. ) ;
#2999 = DIRECTION ( 'NONE',  ( 0.000000000000000000, 0.000000000000000000, 1.000000000000000000 ) ) ;
#3000 = CARTESIAN_POINT ( 'NONE',  ( 2.931639317407903178, -4.080919942823946656, -0.01465562841809697585 ) ) ;
#3001 = APPLICATION_CONTEXT ( 'automotive_design' ) ;
#3002 = CIRCLE ( 'NONE', #12331, 4.000000000000004441 ) ;
#3003 = VERTEX_POINT ( 'NONE', #12232 ) ;
#3004 = ORIENTED_EDGE ( 'NONE', *, *, #3700, .F. ) ;
#3005 = B_SPLINE_CURVE_WITH_KNOTS ( 'NONE', 3,
 ( #14462, #7788, #3630, #9094, #44, #13512 ),
 .UNSPECIFIED., .F., .F.,
 ( 4, 2, 4 ),
 ( 0.000000000000000000, 0.002086519881787259750, 0.004173039763574519501 ),
 .UNSPECIFIED. ) ;
#3006 = DIRECTION ( 'NONE',  ( 0.7071067811865483499, 0.7071067811865467956, -0.000000000000000000 ) ) ;
#3007 = ORIENTED_EDGE ( 'NONE', *, *, #10626, .F. ) ;
#3008 = EDGE_CURVE ( 'NONE', #3564, #13574, #5345, .T. ) ;
#3009 = ORIENTED_EDGE ( 'NONE', *, *, #12007, .F. ) ;
#3010 = DIRECTION ( 'NONE',  ( -0.9701425001453325425, -0.2425356250363304988, 0.000000000000000000 ) ) ;
#3011 = CARTESIAN_POINT ( 'NONE',  ( 62.10586122665989706, -20.42344490663939993, 33.00000000000000000 ) ) ;
#3012 = CIRCLE ( 'NONE', #175, 2.500000000000002220 ) ;
#3013 = CARTESIAN_POINT ( 'NONE',  ( 2.647226096189656985, 48.05180945724377750, 0.9903388192220060615 ) ) ;
#3014 = DIRECTION ( 'NONE',  ( -1.446433017903773725E-17, -0.5000000000000003331, 0.8660254037844383745 ) ) ;
#3015 = CIRCLE ( 'NONE', #12342, 4.000000000000000000 ) ;
#3016 = DIRECTION ( 'NONE',  ( -1.000000000000000000, 0.000000000000000000, 0.000000000000000000 ) ) ;
#3017 = APPLICATION_PROTOCOL_DEFINITION ( 'draft international standard', 'automotive_design', 1998, #5115 ) ;
#3018 = CARTESIAN_POINT ( 'NONE',  ( 0.000000000000000000, 25.49999999999996803, 8.000000000000007105 ) ) ;
#3019 = DIRECTION ( 'NONE',  ( 0.000000000000000000, 0.000000000000000000, 1.000000000000000000 ) ) ;
#3020 = ORIENTED_EDGE ( 'NONE', *, *, #11613, .T. ) ;
#3021 = CONICAL_SURFACE ( 'NONE', #6492, 6.438111078829122036, 1.221730476396037712 ) ;
#3022 = CARTESIAN_POINT ( 'NONE',  ( 108.6817075744280174, 69.57655509336049704, 3.300000000000013589 ) ) ;
#3023 = ORIENTED_EDGE ( 'NONE', *, *, #10591, .F. ) ;
#3024 = AXIS2_PLACEMENT_3D ( 'NONE', #1105, #8786, #8854 ) ;
#3025 = EDGE_LOOP ( 'NONE', ( #1385, #3637, #7202, #9943 ) ) ;
#3026 = AXIS2_PLACEMENT_3D ( 'NONE', #9923, #3139, #9633 ) ;
#3027 = EDGE_CURVE ( 'NONE', #630, #10570, #3438, .T. ) ;
#3028 = ORIENTED_EDGE ( 'NONE', *, *, #3297, .T. ) ;
#3029 = FACE_OUTER_BOUND ( 'NONE', #9225, .T. ) ;
#3030 = FACE_BOUND ( 'NONE', #12290, .T. ) ;
#3031 =( NAMED_UNIT ( * ) SI_UNIT ( $, .STERADIAN. ) SOLID_ANGLE_UNIT ( ) );
#3032 = VERTEX_POINT ( 'NONE', #13257 ) ;
#3033 = B_SPLINE_CURVE_WITH_KNOTS ( 'NONE', 3,
 ( #13828, #12497, #4880, #13751, #9341 ),
 .UNSPECIFIED., .F., .F.,
 ( 4, 1, 4 ),
 ( 6.279784878834692592E-20, 0.002886751345948135490, 0.005773502691896270980 ),
 .UNSPECIFIED. ) ;
#3034 = VERTEX_POINT ( 'NONE', #10023 ) ;
#3035 = CARTESIAN_POINT ( 'NONE',  ( 13.00000000000000533, 29.99999999999999289, 0.000000000000000000 ) ) ;
#3036 = CARTESIAN_POINT ( 'NONE',  ( 4.000000000000004441, 1.563622288139198568, -0.2253451193528359653 ) ) ;
#3037 = DIRECTION ( 'NONE',  ( 0.000000000000000000, 0.000000000000000000, 1.000000000000000000 ) ) ;
#3038 = EDGE_LOOP ( 'NONE', ( #1547, #11800, #11167, #13440 ) ) ;
#3039 = ADVANCED_FACE ( 'NONE', ( #10097 ), #6654, .T. ) ;
#3040 = ADVANCED_FACE ( 'NONE', ( #4417 ), #1030, .F. ) ;
#3041 = DIRECTION ( 'NONE',  ( 0.000000000000000000, 0.000000000000000000, -1.000000000000000000 ) ) ;
#3042 = CARTESIAN_POINT ( 'NONE',  ( -118.6817075744281595, 69.57655509336026967, 3.299999999999982947 ) ) ;
#3043 = LINE ( 'NONE', #4073, #9736 ) ;
#3044 = EDGE_LOOP ( 'NONE', ( #7104, #6788, #3440, #2095 ) ) ;
#3045 = CARTESIAN_POINT ( 'NONE',  ( 5.000000000000001776, 2.886751345948120662, -4.284345921091780696 ) ) ;
#3046 = CARTESIAN_POINT ( 'NONE',  ( 4.862825178850999741, 1.624847281681430111, -4.000000000000002665 ) ) ;
#3047 = VECTOR ( 'NONE', #7306, 1000.000000000000000 ) ;
#3048 = DIRECTION ( 'NONE',  ( -0.000000000000000000, -0.000000000000000000, -1.000000000000000000 ) ) ;
#3049 = EDGE_LOOP ( 'NONE', ( #7279, #7569, #10044, #185 ) ) ;
#3050 = VERTEX_POINT ( 'NONE', #3311 ) ;
#3051 = DIRECTION ( 'NONE',  ( 0.000000000000000000, 0.000000000000000000, 1.000000000000000000 ) ) ;
#3052 = CARTESIAN_POINT ( 'NONE',  ( 1.257202807339443673, -3.892955774273464620, -3.133250573521783267 ) ) ;
#3053 = VECTOR ( 'NONE', #11999, 1000.000000000000000 ) ;
#3054 = ORIENTED_EDGE ( 'NONE', *, *, #13277, .F. ) ;
#3055 = CARTESIAN_POINT ( 'NONE',  ( 3.065261730689029740, 7.410293710401357536, 0.000000000000000000 ) ) ;
#3056 = CARTESIAN_POINT ( 'NONE',  ( 139.9999999999996874, 199.5765550933606107, 47.99999999999998579 ) ) ;
#3057 = ORIENTED_EDGE ( 'NONE', *, *, #9773, .F. ) ;
#3058 = ORIENTED_EDGE ( 'NONE', *, *, #8113, .F. ) ;
#3059 = DIRECTION ( 'NONE',  ( -1.000000000000000000, 0.000000000000000000, 1.387778780781446415E-16 ) ) ;
#3060 = DIRECTION ( 'NONE',  ( 1.000000000000000000, 0.000000000000000000, 0.000000000000000000 ) ) ;
#3061 = VERTEX_POINT ( 'NONE', #7752 ) ;
#3062 = LINE ( 'NONE', #1739, #6317 ) ;
#3063 = CARTESIAN_POINT ( 'NONE',  ( 0.000000000000000000, 25.49999999999996803, 0.000000000000000000 ) ) ;
#3064 = VECTOR ( 'NONE', #10854, 1000.000000000000000 ) ;
#3065 = DIRECTION ( 'NONE',  ( 1.000000000000000000, 0.000000000000000000, 0.000000000000000000 ) ) ;
#3066 = DIRECTION ( 'NONE',  ( 0.000000000000000000, 0.000000000000000000, -1.000000000000000000 ) ) ;
#3067 = VERTEX_POINT ( 'NONE', #11123 ) ;
#3068 =( NAMED_UNIT ( * ) SI_UNIT ( $, .STERADIAN. ) SOLID_ANGLE_UNIT ( ) );
#3069 = CARTESIAN_POINT ( 'NONE',  ( 2.369999999999996998, 4.749999999999999112, 0.000000000000000000 ) ) ;
#3070 = DIRECTION ( 'NONE',  ( 0.000000000000000000, 0.000000000000000000, 1.000000000000000000 ) ) ;
#3071 =( GEOMETRIC_REPRESENTATION_CONTEXT ( 3 ) GLOBAL_UNCERTAINTY_ASSIGNED_CONTEXT ( ( #3983 ) ) GLOBAL_UNIT_ASSIGNED_CONTEXT ( ( #11535, #10370, #9264 ) ) REPRESENTATION_CONTEXT ( 'NONE', 'WORKASPACE' ) );
#3072 = AXIS2_PLACEMENT_3D ( 'NONE', #2513, #1409, #5858 ) ;
#3073 = EDGE_LOOP ( 'NONE', ( #9571, #1894, #9487, #3953 ) ) ;
#3074 = VECTOR ( 'NONE', #9897, 1000.000000000000000 ) ;
#3075 = ORIENTED_EDGE ( 'NONE', *, *, #14001, .T. ) ;
#3076 = EDGE_CURVE ( 'NONE', #1865, #9330, #1098, .T. ) ;
#3077 = PLANE ( 'NONE',  #3142 ) ;
#3078 = EDGE_LOOP ( 'NONE', ( #2383, #8611, #358, #12585, #5861, #6644 ) ) ;
#3079 = ORIENTED_EDGE ( 'NONE', *, *, #3769, .F. ) ;
#3080 = DIRECTION ( 'NONE',  ( -1.000000000000000000, -1.723842398015259277E-15, 0.000000000000000000 ) ) ;
#3081 = LINE ( 'NONE', #13240, #10258 ) ;
#3082 = DIRECTION ( 'NONE',  ( 0.2425356250363328026, -0.9701425001453319874, -0.000000000000000000 ) ) ;
#3083 = AXIS2_PLACEMENT_3D ( 'NONE', #5415, #13414, #12230 ) ;
#3084 = PLANE ( 'NONE',  #4411 ) ;
#3085 = VECTOR ( 'NONE', #9927, 1000.000000000000000 ) ;
#3086 = LINE ( 'NONE', #5048, #14071 ) ;
#3087 = PRODUCT_CONTEXT ( 'NONE', #9795, 'mechanical' ) ;
#3088 = CARTESIAN_POINT ( 'NONE',  ( 3.999999999999998224, 1.680235903636351003, -3.016633206402824730 ) ) ;
#3089 = AXIS2_PLACEMENT_3D ( 'NONE', #8497, #10767, #11719 ) ;
#3090 = CARTESIAN_POINT ( 'NONE',  ( 108.6817075744280174, 109.5765550933605113, -3.299999999999986500 ) ) ;
#3091 = EDGE_CURVE ( 'NONE', #6663, #9400, #11140, .T. ) ;
#3092 = CARTESIAN_POINT ( 'NONE',  ( 22.00000000000000355, 30.00000000000000711, 25.00000000000000000 ) ) ;
#3093 = CIRCLE ( 'NONE', #8680, 2.499999999999999112 ) ;
#3094 = CIRCLE ( 'NONE', #3782, 2.500000000000000444 ) ;
#3095 = ADVANCED_FACE ( 'NONE', ( #13196 ), #7597, .T. ) ;
#3096 = ORIENTED_EDGE ( 'NONE', *, *, #7792, .T. ) ;
#3097 = VERTEX_POINT ( 'NONE', #8992 ) ;
#3098 = DIRECTION ( 'NONE',  ( 0.000000000000000000, 0.000000000000000000, -1.000000000000000000 ) ) ;
#3099 = CYLINDRICAL_SURFACE ( 'NONE', #10041, 3.299999999999997158 ) ;
#3100 = LINE ( 'NONE', #13255, #13131 ) ;
#3101 = VECTOR ( 'NONE', #1062, 1000.000000000000000 ) ;
#3102 = ORIENTED_EDGE ( 'NONE', *, *, #10316, .T. ) ;
#3103 = AXIS2_PLACEMENT_3D ( 'NONE', #14152, #616, #4062 ) ;
#3104 = VECTOR ( 'NONE', #9548, 1000.000000000000000 ) ;
#3105 = LINE ( 'NONE', #13262, #13062 ) ;
#3106 = ADVANCED_FACE ( 'NONE', ( #5692 ), #13480, .F. ) ;
#3107 = DIRECTION ( 'NONE',  ( 1.000000000000000000, 3.286707217423839940E-17, 2.273843122241288053E-18 ) ) ;
#3108 = DIRECTION ( 'NONE',  ( -1.000000000000000000, 0.000000000000000000, 0.000000000000000000 ) ) ;
#3109 = ADVANCED_FACE ( 'NONE', ( #12370 ), #6800, .F. ) ;
#3110 = VECTOR ( 'NONE', #3603, 1000.000000000000000 ) ;
#3111 = CARTESIAN_POINT ( 'NONE',  ( 129.3408537872138595, 189.5765550933606107, -80.00000000000002842 ) ) ;
#3112 = CARTESIAN_POINT ( 'NONE',  ( 5.236872748402768174, 0.5087250997262710017, -4.357689166958468086 ) ) ;
#3113 = PLANE ( 'NONE',  #5740 ) ;
#3114 = DIRECTION ( 'NONE',  ( 0.000000000000000000, 0.000000000000000000, 1.000000000000000000 ) ) ;
#3115 = CARTESIAN_POINT ( 'NONE',  ( 4.873320210002471953, 0.8266591206104413336, -4.072408155786487960 ) ) ;
#3116 =( NAMED_UNIT ( * ) SI_UNIT ( $, .STERADIAN. ) SOLID_ANGLE_UNIT ( ) );
#3117 = CARTESIAN_POINT ( 'NONE',  ( 36.99999999999999289, 80.00000000000000000, 25.00000000000000000 ) ) ;
#3118 = VERTEX_POINT ( 'NONE', #5219 ) ;
#3119 = ORIENTED_EDGE ( 'NONE', *, *, #12620, .F. ) ;
#3120 = CARTESIAN_POINT ( 'NONE',  ( 88.22284556172391490, -83.66032599071898801, -28.00000000000000000 ) ) ;
#3121 = PRESENTATION_LAYER_ASSIGNMENT (  '', '', ( #12930 ) ) ;
#3122 = ADVANCED_FACE ( 'NONE', ( #7255 ), #6077, .F. ) ;
#3123 = AXIS2_PLACEMENT_3D ( 'NONE', #9081, #6607, #3411 ) ;
#3124 = EDGE_CURVE ( 'NONE', #14315, #2424, #1093, .T. ) ;
#3125 = CARTESIAN_POINT ( 'NONE',  ( 0.6641139335914896247, -4.471067008845462709, -3.302142222888722500 ) ) ;
#3126 = ORIENTED_EDGE ( 'NONE', *, *, #2085, .F. ) ;
#3127 = FACE_OUTER_BOUND ( 'NONE', #11935, .T. ) ;
#3128 = CARTESIAN_POINT ( 'NONE',  ( 6.118061346828462449E-15, -30.42344490663947809, -117.0000000000000000 ) ) ;
#3129 = ORIENTED_EDGE ( 'NONE', *, *, #10296, .F. ) ;
#3130 = EDGE_LOOP ( 'NONE', ( #2759, #11816, #4750, #10395, #6166 ) ) ;
#3131 = EDGE_LOOP ( 'NONE', ( #7315, #5168, #9079, #14380, #126, #4095, #11671, #3360, #2498, #9694, #10895, #5389 ) ) ;
#3132 = CARTESIAN_POINT ( 'NONE',  ( 22.00000000000000000, 60.00000000000000711, -25.00000000000000000 ) ) ;
#3133 = CARTESIAN_POINT ( 'NONE',  ( 44.55443476855437268, 62.09002498982675888, 25.00000000000000000 ) ) ;
#3134 = VECTOR ( 'NONE', #243, 1000.000000000000000 ) ;
#3135 = ORIENTED_EDGE ( 'NONE', *, *, #6230, .F. ) ;
#3136 = CARTESIAN_POINT ( 'NONE',  ( 3.950241966888157652, -2.668221755853173338, -2.378504353001417826 ) ) ;
#3137 = CONICAL_SURFACE ( 'NONE', #14122, 2.055000000000000160, 0.7853981633974428389 ) ;
#3138 = CARTESIAN_POINT ( 'NONE',  ( -0.3198814748697705879, -4.434118497892186817, -0.3507732604232561280 ) ) ;
#3139 = DIRECTION ( 'NONE',  ( 0.000000000000000000, -0.8660254037844388186, -0.4999999999999998335 ) ) ;
#3140 = DIRECTION ( 'NONE',  ( 0.000000000000000000, -1.000000000000000000, 0.000000000000000000 ) ) ;
#3141 = SURFACE_STYLE_FILL_AREA ( #4240 ) ;
#3142 = AXIS2_PLACEMENT_3D ( 'NONE', #6413, #3006, #7436 ) ;
#3143 = DIRECTION ( 'NONE',  ( -1.000000000000000000, -0.000000000000000000, -0.000000000000000000 ) ) ;
#3144 = EDGE_CURVE ( 'NONE', #5297, #4481, #12833, .T. ) ;
#3145 = CARTESIAN_POINT ( 'NONE',  ( 0.000000000000000000, 0.000000000000000000, 13.31572692736082786 ) ) ;
#3146 = AXIS2_PLACEMENT_3D ( 'NONE', #2793, #3667, #13770 ) ;
#3147 = ORIENTED_EDGE ( 'NONE', *, *, #14087, .T. ) ;
#3148 = CARTESIAN_POINT ( 'NONE',  ( 4.597743007729421905, 3.118994528718957771, -0.4198507760575558301 ) ) ;
#3149 = ORIENTED_EDGE ( 'NONE', *, *, #9166, .T. ) ;
#3150 = CYLINDRICAL_SURFACE ( 'NONE', #6770, 3.299999999999976730 ) ;
#3151 = CARTESIAN_POINT ( 'NONE',  ( 0.000000000000000000, -4.618802153517030717, -3.133295621305376422 ) ) ;
#3152 = CARTESIAN_POINT ( 'NONE',  ( 3.973178806327566370, 47.44387873568884118, 4.532639216498019152 ) ) ;
#3153 = CARTESIAN_POINT ( 'NONE',  ( 108.6817075744280459, 109.5765550933604828, -3.299999999999976730 ) ) ;
#3154 = CARTESIAN_POINT ( 'NONE',  ( 4.175813232069169878, 4.122719923832743660, 0.000000000000000000 ) ) ;
#3155 = PRODUCT_CONTEXT ( 'NONE', #2890, 'mechanical' ) ;
#3156 = CARTESIAN_POINT ( 'NONE',  ( 3.999999999999998224, -0.8732118962410245766, -2.923153487222556191 ) ) ;
#3157 = DIRECTION ( 'NONE',  ( -0.000000000000000000, -1.000000000000000000, 0.000000000000000000 ) ) ;
#3158 = ADVANCED_FACE ( 'NONE', ( #12917 ), #13061, .F. ) ;
#3159 = ADVANCED_FACE ( 'NONE', ( #11654 ), #14158, .F. ) ;
#3160 = DIRECTION ( 'NONE',  ( 1.000000000000000000, 0.000000000000000000, 0.000000000000000000 ) ) ;
#3161 = ORIENTED_EDGE ( 'NONE', *, *, #356, .T. ) ;
#3162 = EDGE_CURVE ( 'NONE', #373, #1264, #3043, .T. ) ;
#3163 = CARTESIAN_POINT ( 'NONE',  ( 129.3408537872138595, 189.5765550933606107, -69.99999999999998579 ) ) ;
#3164 = B_SPLINE_CURVE_WITH_KNOTS ( 'NONE', 3,
 ( #9605, #4071, #12093, #9685, #821, #4289 ),
 .UNSPECIFIED., .F., .F.,
 ( 4, 2, 4 ),
 ( -3.988673288087340225E-06, 0.0002483701411510689508, 0.0005007289555902253103 ),
 .UNSPECIFIED. ) ;
#3165 = CARTESIAN_POINT ( 'NONE',  ( 20.00000000000000000, -5.510910596163090344E-15, -25.00000000000000000 ) ) ;
#3166 = SURFACE_STYLE_USAGE ( .BOTH. , #3232 ) ;
#3167 = EDGE_CURVE ( 'NONE', #2838, #1176, #544, .T. ) ;
#3168 = LINE ( 'NONE', #13195, #7244 ) ;
#3169 = DIRECTION ( 'NONE',  ( -1.000000000000000000, 0.000000000000000000, -0.000000000000000000 ) ) ;
#3170 = VERTEX_POINT ( 'NONE', #8352 ) ;
#3171 = ADVANCED_FACE ( 'NONE', ( #5288 ), #5007, .T. ) ;
#3172 = EDGE_CURVE ( 'NONE', #14042, #12296, #5144, .T. ) ;
#3173 = CARTESIAN_POINT ( 'NONE',  ( 22.00000000000000355, 37.00000000000000711, 25.00000000000000000 ) ) ;
#3174 = LINE ( 'NONE', #2219, #6591 ) ;
#3175 = CARTESIAN_POINT ( 'NONE',  ( 1.560000000000005826, 1.732050807568871864, 0.000000000000000000 ) ) ;
#3176 = CARTESIAN_POINT ( 'NONE',  ( -3.472352378023202846, -2.614038573344081406, -3.020318136128327335 ) ) ;
#3177 = CARTESIAN_POINT ( 'NONE',  ( -5.000000000000001776, -2.886751345948141534, -6.000000000000005329 ) ) ;
#3178 = CARTESIAN_POINT ( 'NONE',  ( 8.000000000000000000, 25.49999999999996803, 8.000000000000007105 ) ) ;
#3179 = LINE ( 'NONE', #8860, #850 ) ;
#3180 = EDGE_CURVE ( 'NONE', #3412, #1341, #11596, .T. ) ;
#3181 = CARTESIAN_POINT ( 'NONE',  ( 4.175813232069169878, -2.061359961916364725, 3.570380186727409200 ) ) ;
#3182 = LINE ( 'NONE', #6311, #1111 ) ;
#3183 = FACE_OUTER_BOUND ( 'NONE', #4456, .T. ) ;
#3184 = VERTEX_POINT ( 'NONE', #10782 ) ;
#3185 = ORIENTED_EDGE ( 'NONE', *, *, #8957, .T. ) ;
#3186 = CARTESIAN_POINT ( 'NONE',  ( 39.70372226782770753, 81.49287499273339108, -25.00000000000000000 ) ) ;
#3187 = B_SPLINE_CURVE_WITH_KNOTS ( 'NONE', 3,
 ( #13292, #3268, #782, #2987, #7707 ),
 .UNSPECIFIED., .F., .F.,
 ( 4, 1, 4 ),
 ( 0.000000000000000000, 0.002020725942163690073, 0.004041451884327380145 ),
 .UNSPECIFIED. ) ;
#3188 = FACE_OUTER_BOUND ( 'NONE', #10770, .T. ) ;
#3189 = ORIENTED_EDGE ( 'NONE', *, *, #418, .T. ) ;
#3190 = DIRECTION ( 'NONE',  ( 1.734723475976770502E-18, -4.440892098500621231E-16, -1.000000000000000000 ) ) ;
#3191 = FACE_BOUND ( 'NONE', #14002, .T. ) ;
#3192 = VERTEX_POINT ( 'NONE', #14017 ) ;
#3193 = VERTEX_POINT ( 'NONE', #691 ) ;
#3194 = ORIENTED_EDGE ( 'NONE', *, *, #2487, .F. ) ;
#3195 = CARTESIAN_POINT ( 'NONE',  ( 4.207491450040564906, -2.029819825146478074, -3.371670828759588012 ) ) ;
#3196 = LINE ( 'NONE', #11906, #12910 ) ;
#3197 = EDGE_CURVE ( 'NONE', #5783, #630, #4084, .T. ) ;
#3198 = CARTESIAN_POINT ( 'NONE',  ( 22.00000000000000000, 70.00000000000000000, -25.00000000000000000 ) ) ;
#3199 = FACE_OUTER_BOUND ( 'NONE', #14336, .T. ) ;
#3200 = DIRECTION ( 'NONE',  ( 0.000000000000000000, 0.000000000000000000, 1.000000000000000000 ) ) ;
#3201 = DIRECTION ( 'NONE',  ( 0.000000000000000000, -0.000000000000000000, -1.000000000000000000 ) ) ;
#3202 = ORIENTED_EDGE ( 'NONE', *, *, #14383, .T. ) ;
#3203 = CARTESIAN_POINT ( 'NONE',  ( -3.000000000000000888, 3.469446951953614189E-15, -5.974599999999997024 ) ) ;
#3204 = CARTESIAN_POINT ( 'NONE',  ( 57.35294117647057277, -1.411764705882362358, -23.00000000000000000 ) ) ;
#3205 = DIRECTION ( 'NONE',  ( -0.9240638205168504316, -0.3822382184081047352, 0.000000000000000000 ) ) ;
#3206 = VECTOR ( 'NONE', #10561, 1000.000000000000000 ) ;
#3207 = EDGE_LOOP ( 'NONE', ( #7908, #5778 ) ) ;
#3208 = ORIENTED_EDGE ( 'NONE', *, *, #11066, .T. ) ;
#3209 = FACE_OUTER_BOUND ( 'NONE', #14027, .T. ) ;
#3210 = EDGE_CURVE ( 'NONE', #7073, #12268, #11811, .T. ) ;
#3211 = ORIENTED_EDGE ( 'NONE', *, *, #868, .F. ) ;
#3212 = CARTESIAN_POINT ( 'NONE',  ( 3.950233766685595338, 0.7256672287185880199, -3.500000000000147882 ) ) ;
#3213 = EDGE_CURVE ( 'NONE', #716, #5014, #4141, .T. ) ;
#3214 = CARTESIAN_POINT ( 'NONE',  ( 92.68170757442806007, 124.5765550933605965, 25.00000000000000000 ) ) ;
#3215 = B_SPLINE_CURVE_WITH_KNOTS ( 'NONE', 3,
 ( #443, #3886, #10236, #11625, #4896, #7080 ),
 .UNSPECIFIED., .F., .F.,
 ( 4, 2, 4 ),
 ( 0.003805861006858111961, 0.004828937052660012795, 0.005852013098461913629 ),
 .UNSPECIFIED. ) ;
#3216 = CARTESIAN_POINT ( 'NONE',  ( 3.010143253645308992, 47.91462539009204136, 1.353322078536349338 ) ) ;
#3217 = LINE ( 'NONE', #4470, #10464 ) ;
#3218 = CARTESIAN_POINT ( 'NONE',  ( 6.800000000000028244, 2.309401076758504701, -4.000000000000003553 ) ) ;
#3219 = ITEM_DEFINED_TRANSFORMATION ( 'NONE', 'NONE', #7088,  #11025 ) ;
#3220 = CARTESIAN_POINT ( 'NONE',  ( 3.999999999999999112, -2.511476383524243072, -3.169254053377029923 ) ) ;
#3221 = CARTESIAN_POINT ( 'NONE',  ( 5.103279350327408537, -4.707503328691831967, 2.873572379795871114E-14 ) ) ;
#3222 = VECTOR ( 'NONE', #5160, 1000.000000000000000 ) ;
#3223 = ORIENTED_EDGE ( 'NONE', *, *, #1236, .T. ) ;
#3224 = LINE ( 'NONE', #869, #9413 ) ;
#3225 = VERTEX_POINT ( 'NONE', #9607 ) ;
#3226 = DIRECTION ( 'NONE',  ( -1.000000000000000000, 1.892425610156516875E-16, 0.000000000000000000 ) ) ;
#3227 = CIRCLE ( 'NONE', #7674, 3.000000000000003553 ) ;
#3228 = ORIENTED_EDGE ( 'NONE', *, *, #14154, .T. ) ;
#3229 = CIRCLE ( 'NONE', #9295, 3.000000000000000888 ) ;
#3230 = PLANE ( 'NONE',  #3954 ) ;
#3231 = CARTESIAN_POINT ( 'NONE',  ( -5.000000000000000000, 1.231908430319618164, -0.1119772403577083270 ) ) ;
#3232 = SURFACE_SIDE_STYLE ('',( #11050 ) ) ;
#3233 = DIRECTION ( 'NONE',  ( 0.000000000000000000, 1.000000000000000000, 1.224646799147353207E-16 ) ) ;
#3234 = ORIENTED_EDGE ( 'NONE', *, *, #8785, .F. ) ;
#3235 = CARTESIAN_POINT ( 'NONE',  ( 22.00000000000000355, 50.00000000000000000, 25.00000000000000000 ) ) ;
#3236 = LINE ( 'NONE', #7826, #6818 ) ;
#3237 = SHAPE_REPRESENTATION_RELATIONSHIP ( 'NONE' , 'NONE' ,  #8883, #13802 ) ;
#3238 = CARTESIAN_POINT ( 'NONE',  ( 23.40000000000000213, 29.99999999999999645, -24.99999999999999289 ) ) ;
#3239 = ORIENTED_EDGE ( 'NONE', *, *, #4906, .T. ) ;
#3240 = VECTOR ( 'NONE', #7916, 1000.000000000000114 ) ;
#3241 = CARTESIAN_POINT ( 'NONE',  ( 108.6817075744280316, -30.42344490663958112, -32.00000000000002842 ) ) ;
#3242 = LINE ( 'NONE', #13202, #3805 ) ;
#3243 = EDGE_CURVE ( 'NONE', #7740, #12547, #14228, .T. ) ;
#3244 = CARTESIAN_POINT ( 'NONE',  ( 22.00000000000000000, 57.00000000000000000, 25.00000000000000000 ) ) ;
#3245 = VERTEX_POINT ( 'NONE', #9465 ) ;
#3246 = CARTESIAN_POINT ( 'NONE',  ( -4.175003227304313391, -2.208362916365310902, -3.169254239516198890 ) ) ;
#3247 = EDGE_CURVE ( 'NONE', #5464, #6880, #7148, .T. ) ;
#3248 = CARTESIAN_POINT ( 'NONE',  ( 4.988724804725785944, -4.618802153517009401, 0.000000000000000000 ) ) ;
#3249 = PLANE ( 'NONE',  #7377 ) ;
#3250 = CARTESIAN_POINT ( 'NONE',  ( 139.9999999999996874, 189.5765550933606107, 47.99999999999998579 ) ) ;
#3251 = EDGE_CURVE ( 'NONE', #14451, #5279, #3179, .T. ) ;
#3252 = CARTESIAN_POINT ( 'NONE',  ( 31.24550000000003536, 1.332267629550187849E-15, 3.000000000000003553 ) ) ;
#3253 = LINE ( 'NONE', #9903, #5813 ) ;
#3254 = LINE ( 'NONE', #9693, #13621 ) ;
#3255 = VERTEX_POINT ( 'NONE', #8652 ) ;
#3256 = DIRECTION ( 'NONE',  ( 1.000000000000000000, 3.286707217423839940E-17, 2.273843122241288053E-18 ) ) ;
#3257 = SURFACE_SIDE_STYLE ('',( #13363 ) ) ;
#3258 = ORIENTED_EDGE ( 'NONE', *, *, #12743, .T. ) ;
#3259 = CARTESIAN_POINT ( 'NONE',  ( 20.00000000000000000, -5.510910596163090344E-15, -25.00000000000000000 ) ) ;
#3260 = EDGE_CURVE ( 'NONE', #6812, #6602, #2734, .T. ) ;
#3261 = DIRECTION ( 'NONE',  ( -1.000000000000000000, -0.000000000000000000, -0.000000000000000000 ) ) ;
#3262 = VECTOR ( 'NONE', #14029, 1000.000000000000000 ) ;
#3263 = ORIENTED_EDGE ( 'NONE', *, *, #12673, .F. ) ;
#3264 = ORIENTED_EDGE ( 'NONE', *, *, #9653, .F. ) ;
#3265 = EDGE_LOOP ( 'NONE', ( #10728, #1907, #5085, #7095 ) ) ;
#3266 = AXIS2_PLACEMENT_3D ( 'NONE', #6986, #8974, #5731 ) ;
#3267 = EDGE_CURVE ( 'NONE', #11002, #4176, #11363, .T. ) ;
#3268 = CARTESIAN_POINT ( 'NONE',  ( 3.951447005078475350, 1.347150628109120563, -3.499999999999995559 ) ) ;
#3269 = DIRECTION ( 'NONE',  ( 0.000000000000000000, 0.000000000000000000, 1.000000000000000000 ) ) ;
#3270 = CARTESIAN_POINT ( 'NONE',  ( 4.158806965674308742, -1.986429158307094101, -3.559403772175848690 ) ) ;
#3271 = CARTESIAN_POINT ( 'NONE',  ( -3.679171394226031122, -2.494631558665846516, -0.3503314178412552105 ) ) ;
#3272 = CARTESIAN_POINT ( 'NONE',  ( 105.6817075744280174, 69.57655509336049704, -3.299999999999981171 ) ) ;
#3273 = FACE_OUTER_BOUND ( 'NONE', #7493, .T. ) ;
#3274 = EDGE_LOOP ( 'NONE', ( #4705, #5728, #11239 ) ) ;
#3275 = SURFACE_STYLE_USAGE ( .BOTH. , #1140 ) ;
#3276 = AXIS2_PLACEMENT_3D ( 'NONE', #2865, #2360, #3959 ) ;
#3277 = CARTESIAN_POINT ( 'NONE',  ( 5.103531824934171013, 4.708196996972911386, -1.387778780781445676E-14 ) ) ;
#3278 = AXIS2_PLACEMENT_3D ( 'NONE', #8415, #9670, #13047 ) ;
#3279 = CARTESIAN_POINT ( 'NONE',  ( 4.158921614371303477, 4.076055977742297110, -0.05993604794451207196 ) ) ;
#3280 = ADVANCED_FACE ( 'NONE', ( #13207 ), #11072, .T. ) ;
#3281 = ORIENTED_EDGE ( 'NONE', *, *, #3284, .T. ) ;
#3282 = ORIENTED_EDGE ( 'NONE', *, *, #13778, .F. ) ;
#3283 = LINE ( 'NONE', #14192, #3834 ) ;
#3284 = EDGE_CURVE ( 'NONE', #4075, #3991, #13253, .T. ) ;
#3285 = VERTEX_POINT ( 'NONE', #10039 ) ;
#3286 = CARTESIAN_POINT ( 'NONE',  ( 27.75000000000001066, 0.000000000000000000, 0.000000000000000000 ) ) ;
#3287 = LINE ( 'NONE', #8693, #6049 ) ;
#3288 = LINE ( 'NONE', #12492, #11902 ) ;
#3289 = CARTESIAN_POINT ( 'NONE',  ( 5.000000000000000000, -2.886751345948152192, -0.5999999999999894307 ) ) ;
#3290 = CARTESIAN_POINT ( 'NONE',  ( 20.00000000000000000, 27.00000000000000355, 25.00000000000000000 ) ) ;
#3291 = CONTEXT_DEPENDENT_SHAPE_REPRESENTATION ( #10249, #6943 ) ;
#3292 = CARTESIAN_POINT ( 'NONE',  ( -13.00000000000000533, 29.99999999999999289, 0.000000000000000000 ) ) ;
#3293 = CARTESIAN_POINT ( 'NONE',  ( 4.114405500665256454, 2.025575754679707963, -3.508400121684933204 ) ) ;
#3294 = CIRCLE ( 'NONE', #12398, 5.000000000000000888 ) ;
#3295 = AXIS2_PLACEMENT_3D ( 'NONE', #10853, #2740, #14161 ) ;
#3296 = EDGE_LOOP ( 'NONE', ( #5557, #14094 ) ) ;
#3297 = EDGE_CURVE ( 'NONE', #696, #1781, #12095, .T. ) ;
#3298 = EDGE_CURVE ( 'NONE', #4830, #14165, #2069, .T. ) ;
#3299 = CARTESIAN_POINT ( 'NONE',  ( 4.686019787951574145, 3.464101615137745060, 2.000000000000011990 ) ) ;
#3300 = ORIENTED_EDGE ( 'NONE', *, *, #12821, .T. ) ;
#3301 = DIRECTION ( 'NONE',  ( 0.000000000000000000, 0.000000000000000000, 1.000000000000000000 ) ) ;
#3302 = ORIENTED_EDGE ( 'NONE', *, *, #8010, .T. ) ;
#3303 = VECTOR ( 'NONE', #3585, 1000.000000000000000 ) ;
#3304 = EDGE_LOOP ( 'NONE', ( #1284, #4695, #387, #6746, #5667 ) ) ;
#3305 = PRESENTATION_STYLE_ASSIGNMENT (( #7665 ) ) ;
#3306 = AXIS2_PLACEMENT_3D ( 'NONE', #9096, #11438, #10137 ) ;
#3307 = CARTESIAN_POINT ( 'NONE',  ( -3.060208875726627031, 4.280211771583977587, -4.357749648769113193 ) ) ;
#3308 = DIRECTION ( 'NONE',  ( 0.9701425001453319874, 0.2425356250363328858, 0.000000000000000000 ) ) ;
#3309 = VECTOR ( 'NONE', #12595, 1000.000000000000000 ) ;
#3310 = DIRECTION ( 'NONE',  ( 1.000000000000000000, 0.000000000000000000, 0.000000000000000000 ) ) ;
#3311 = CARTESIAN_POINT ( 'NONE',  ( 51.83050351964435976, 32.98574998546678927, -25.00000000000000000 ) ) ;
#3312 = DIRECTION ( 'NONE',  ( 0.5000000000000036637, 0.8660254037844365982, -8.404057939144371073E-32 ) ) ;
#3313 = CARTESIAN_POINT ( 'NONE',  ( 0.000000000000000000, 0.000000000000000000, 0.000000000000000000 ) ) ;
#3314 = CARTESIAN_POINT ( 'NONE',  ( -4.000000000000000000, 2.309401076758492266, -3.204269196027521804 ) ) ;
#3315 = ORIENTED_EDGE ( 'NONE', *, *, #1758, .T. ) ;
#3316 = EDGE_LOOP ( 'NONE', ( #4766, #10357, #7339, #6949 ) ) ;
#3317 = CARTESIAN_POINT ( 'NONE',  ( 0.000000000000000000, 0.000000000000000000, 0.000000000000000000 ) ) ;
#3318 = VECTOR ( 'NONE', #670, 1000.000000000000000 ) ;
#3319 = COLOUR_RGB ( '', 0.09019608, 0.27058824, 0.51372549) ;
#3320 = VECTOR ( 'NONE', #4898, 1000.000000000000114 ) ;
#3321 = EDGE_CURVE ( 'NONE', #6195, #10355, #8937, .T. ) ;
#3322 = LINE ( 'NONE', #1039, #12219 ) ;
#3323 = LINE ( 'NONE', #2220, #5450 ) ;
#3324 = ORIENTED_EDGE ( 'NONE', *, *, #4531, .F. ) ;
#3325 = CARTESIAN_POINT ( 'NONE',  ( -3.453019673806352774, -2.625200315326694067, -3.235259548910466076 ) ) ;
#3326 = EDGE_CURVE ( 'NONE', #6044, #2625, #4210, .T. ) ;
#3327 = CARTESIAN_POINT ( 'NONE',  ( 4.769962962078704294, -3.881286623615096687, 1.277414369161164798 ) ) ;
#3328 = DIRECTION ( 'NONE',  ( 0.000000000000000000, 0.000000000000000000, -1.000000000000000000 ) ) ;
#3329 = DIRECTION ( 'NONE',  ( -1.000000000000000000, 2.551526159633733968E-19, 1.987661601597216239E-18 ) ) ;
#3330 = VECTOR ( 'NONE', #3682, 1000.000000000000000 ) ;
#3331 = CARTESIAN_POINT ( 'NONE',  ( 4.175813232069169878, -2.061359961916378492, -3.570380186727409200 ) ) ;
#3332 = ORIENTED_EDGE ( 'NONE', *, *, #2517, .T. ) ;
#3333 = CARTESIAN_POINT ( 'NONE',  ( 22.00000000000000711, 17.00000000000000000, 25.00000000000000000 ) ) ;
#3334 = B_SPLINE_CURVE_WITH_KNOTS ( 'NONE', 3,
 ( #11145, #31, #6827, #7702 ),
 .UNSPECIFIED., .F., .F.,
 ( 4, 4 ),
 ( 2.380739282295133395E-07, 0.002044882221487524538 ),
 .UNSPECIFIED. ) ;
#3335 = ADVANCED_FACE ( 'NONE', ( #6741 ), #3113, .T. ) ;
#3336 = ORIENTED_EDGE ( 'NONE', *, *, #1469, .T. ) ;
#3337 = DIRECTION ( 'NONE',  ( -0.2425356250363328581, 0.9701425001453318764, 0.000000000000000000 ) ) ;
#3338 = CIRCLE ( 'NONE', #13390, 2.499999999999999112 ) ;
#3339 = STYLED_ITEM ( 'NONE', ( #1054 ), #6268 ) ;
#3340 = CARTESIAN_POINT ( 'NONE',  ( 22.28098402457129268, 141.4229888148237251, 28.00000000000000000 ) ) ;
#3341 = VECTOR ( 'NONE', #7973, 1000.000000000000000 ) ;
#3342 = ORIENTED_EDGE ( 'NONE', *, *, #13049, .T. ) ;
#3343 = ORIENTED_EDGE ( 'NONE', *, *, #944, .F. ) ;
#3344 = CARTESIAN_POINT ( 'NONE',  ( -2.999999999999986233, 3.673940397442042119E-16, 5.421010862427522170E-17 ) ) ;
#3345 = DIRECTION ( 'NONE',  ( 0.000000000000000000, 0.000000000000000000, 1.000000000000000000 ) ) ;
#3346 = EDGE_CURVE ( 'NONE', #716, #14013, #7689, .T. ) ;
#3347 = CARTESIAN_POINT ( 'NONE',  ( 19.99999999999999645, 57.00000000000000000, 25.00000000000000000 ) ) ;
#3348 = DIRECTION ( 'NONE',  ( 0.000000000000000000, -1.000000000000000000, 0.000000000000000000 ) ) ;
#3349 = PLANE ( 'NONE',  #440 ) ;
#3350 = ADVANCED_FACE ( 'NONE', ( #6442 ), #4357, .T. ) ;
#3351 = CARTESIAN_POINT ( 'NONE',  ( 3.806834918298607651, -6.505213034913026604E-16, 3.499999999999989342 ) ) ;
#3352 = AXIS2_PLACEMENT_3D ( 'NONE', #14386, #11295, #5779 ) ;
#3353 = ORIENTED_EDGE ( 'NONE', *, *, #4645, .F. ) ;
#3354 = AXIS2_PLACEMENT_3D ( 'NONE', #14003, #8637, #2879 ) ;
#3355 = ORIENTED_EDGE ( 'NONE', *, *, #2716, .F. ) ;
#3356 = DIRECTION ( 'NONE',  ( -1.000000000000000000, 2.551526159633733968E-19, 1.987661601597216239E-18 ) ) ;
#3357 = EDGE_CURVE ( 'NONE', #2898, #4300, #8799, .T. ) ;
#3358 = CARTESIAN_POINT ( 'NONE',  ( 4.052424581287640493, 3.786734753434984668, 0.5771415817956560002 ) ) ;
#3359 = ORIENTED_EDGE ( 'NONE', *, *, #5495, .T. ) ;
#3360 = ORIENTED_EDGE ( 'NONE', *, *, #4681, .F. ) ;
#3361 = CIRCLE ( 'NONE', #12006, 2.500000000000002220 ) ;
#3362 = VERTEX_POINT ( 'NONE', #4435 ) ;
#3363 = CARTESIAN_POINT ( 'NONE',  ( 6.118061346828462449E-15, -30.42344490663947809, 33.00000000000002842 ) ) ;
#3364 = ORIENTED_EDGE ( 'NONE', *, *, #9327, .T. ) ;
#3365 = CARTESIAN_POINT ( 'NONE',  ( 0.000000000000000000, 0.000000000000000000, 0.000000000000000000 ) ) ;
#3366 = B_SPLINE_CURVE_WITH_KNOTS ( 'NONE', 3,
 ( #10630, #10844, #10906, #3978, #2809, #3036, #10775, #9676 ),
 .UNSPECIFIED., .F., .F.,
 ( 4, 2, 2, 4 ),
 ( 0.005725059856848626130, 0.006314084072593611867, 0.006903108288338597603, 0.008081156719828569077 ),
 .UNSPECIFIED. ) ;
#3367 = B_SPLINE_CURVE_WITH_KNOTS ( 'NONE', 3,
 ( #4301, #7780, #8805, #10926, #11081 ),
 .UNSPECIFIED., .F., .F.,
 ( 4, 1, 4 ),
 ( 5.651806390950781813E-20, 0.002886751345948135924, 0.005773502691896271848 ),
 .UNSPECIFIED. ) ;
#3368 = CARTESIAN_POINT ( 'NONE',  ( -5.000000000000000888, 0.000000000000000000, 0.000000000000000000 ) ) ;
#3369 = FACE_OUTER_BOUND ( 'NONE', #6945, .T. ) ;
#3370 = EDGE_CURVE ( 'NONE', #10504, #11904, #6227, .T. ) ;
#3371 = DIRECTION ( 'NONE',  ( -1.000000000000000000, 0.000000000000000000, 0.000000000000000000 ) ) ;
#3372 = ORIENTED_EDGE ( 'NONE', *, *, #4152, .F. ) ;
#3373 = CARTESIAN_POINT ( 'NONE',  ( 108.6817075744280174, 109.5765550933605113, 3.300000000000008260 ) ) ;
#3374 = CARTESIAN_POINT ( 'NONE',  ( 3.999999999999998224, 0.8378468363844258082, -2.920592527564365160 ) ) ;
#3375 = CARTESIAN_POINT ( 'NONE',  ( 5.084394237956035845, -4.671926501058319303, -1.387778780781445676E-14 ) ) ;
#3376 = VECTOR ( 'NONE', #3037, 1000.000000000000000 ) ;
#3377 = CARTESIAN_POINT ( 'NONE',  ( 4.093692494532781723, -2.021783646005765878, 3.501831996793828949 ) ) ;
#3378 = AXIS2_PLACEMENT_3D ( 'NONE', #9933, #7578, #5467 ) ;
#3379 = EDGE_LOOP ( 'NONE', ( #11741, #8124, #10747, #2937 ) ) ;
#3380 = PLANE ( 'NONE',  #13677 ) ;
#3381 =( GEOMETRIC_REPRESENTATION_CONTEXT ( 3 ) GLOBAL_UNCERTAINTY_ASSIGNED_CONTEXT ( ( #307 ) ) GLOBAL_UNIT_ASSIGNED_CONTEXT ( ( #6803, #13337, #12303 ) ) REPRESENTATION_CONTEXT ( 'NONE', 'WORKASPACE' ) );
#3382 = ORIENTED_EDGE ( 'NONE', *, *, #4255, .F. ) ;
#3383 = CARTESIAN_POINT ( 'NONE',  ( 0.000000000000000000, 0.8660254037844428154, 1.500000000000001332 ) ) ;
#3384 = CARTESIAN_POINT ( 'NONE',  ( -4.817220356105915258, 3.279784343982800277, -4.566919140436430880 ) ) ;
#3385 = CARTESIAN_POINT ( 'NONE',  ( 0.000000000000000000, 4.862606272033096033, -3.445885042887453231 ) ) ;
#3386 = EDGE_CURVE ( 'NONE', #8457, #11273, #14423, .T. ) ;
#3387 = CARTESIAN_POINT ( 'NONE',  ( 0.000000000000000000, 0.000000000000000000, -0.3851141460153306717 ) ) ;
#3388 = CARTESIAN_POINT ( 'NONE',  ( 59.18121602037099649, 13.58289998256015352, -25.00000000000000000 ) ) ;
#3389 = CARTESIAN_POINT ( 'NONE',  ( -4.211140560182194292, 2.431303136016534250, -3.445885042887453231 ) ) ;
#3391 = AXIS2_PLACEMENT_3D ( 'NONE', #4664, #7870, #6912 ) ;
#3390 = SURFACE_SIDE_STYLE ('',( #90 ) ) ;
#3392 = CARTESIAN_POINT ( 'NONE',  ( 0.000000000000000000, 0.000000000000000000, -4.699999999999981526 ) ) ;
#3393 = VERTEX_POINT ( 'NONE', #3250 ) ;
#3394 = ORIENTED_EDGE ( 'NONE', *, *, #10742, .T. ) ;
#3395 = DIRECTION ( 'NONE',  ( 0.000000000000000000, 0.000000000000000000, 1.000000000000000000 ) ) ;
#3396 = CARTESIAN_POINT ( 'NONE',  ( 20.00000000000000000, 80.00000000000000000, 25.00000000000000000 ) ) ;
#3397 = CARTESIAN_POINT ( 'NONE',  ( 3.200000000000000622, 5.329070518200750211E-16, 2.400000000000013234 ) ) ;
#3398 = ORIENTED_EDGE ( 'NONE', *, *, #8557, .F. ) ;
#3399 = DIRECTION ( 'NONE',  ( 0.000000000000000000, 0.000000000000000000, 1.000000000000000000 ) ) ;
#3400 = CYLINDRICAL_SURFACE ( 'NONE', #14432, 4.999999999999988454 ) ;
#3401 = DIRECTION ( 'NONE',  ( 1.000000000000000000, 0.000000000000000000, 0.000000000000000000 ) ) ;
#3402 = EDGE_CURVE ( 'NONE', #13672, #4341, #11854, .T. ) ;
#3403 = DIRECTION ( 'NONE',  ( 1.000000000000000000, -0.000000000000000000, -0.000000000000000000 ) ) ;
#3404 = ADVANCED_FACE ( 'NONE', ( #10915 ), #889, .T. ) ;
#3405 = SURFACE_STYLE_USAGE ( .BOTH. , #2430 ) ;
#3406 = B_SPLINE_CURVE_WITH_KNOTS ( 'NONE', 3,
 ( #10752, #5189, #12726, #2713, #7147, #8553, #9511, #11623, #1601, #12798, #515, #1682, #13914, #8400, #12879, #3885 ),
 .UNSPECIFIED., .F., .F.,
 ( 4, 3, 3, 3, 3, 4 ),
 ( -2.214559098585470453E-06, 0.000000000000000000, 3.881464059292277384E-05, 7.921402936568253800E-05, 0.0001155901529638105323, 0.0001522174276056047432 ),
 .UNSPECIFIED. ) ;
#3407 = CARTESIAN_POINT ( 'NONE',  ( 4.988724804725896966, 2.309401076758504701, 4.000000000000031086 ) ) ;
#3408 = ORIENTED_EDGE ( 'NONE', *, *, #3842, .T. ) ;
#3409 = CARTESIAN_POINT ( 'NONE',  ( 139.9999999999996874, 189.5765550933606107, 47.99999999999998579 ) ) ;
#3410 = ORIENTED_EDGE ( 'NONE', *, *, #2855, .T. ) ;
#3411 = DIRECTION ( 'NONE',  ( 1.000000000000000000, 1.665334536937734071E-16, 0.000000000000000000 ) ) ;
#3412 = VERTEX_POINT ( 'NONE', #11452 ) ;
#3413 = ORIENTED_EDGE ( 'NONE', *, *, #213, .T. ) ;
#3414 = DIRECTION ( 'NONE',  ( 0.000000000000000000, 1.000000000000000000, -0.000000000000000000 ) ) ;
#3415 = LINE ( 'NONE', #7626, #2161 ) ;
#3416 = CARTESIAN_POINT ( 'NONE',  ( 31.38313257588138683, 143.6985259526510390, 28.00000000000000000 ) ) ;
#3417 = LINE ( 'NONE', #6613, #4635 ) ;
#3418 = EDGE_CURVE ( 'NONE', #1767, #6248, #10583, .T. ) ;
#3419 = CARTESIAN_POINT ( 'NONE',  ( 22.00000000000000355, 30.00000000000000711, -25.00000000000000000 ) ) ;
#3420 = VERTEX_POINT ( 'NONE', #13891 ) ;
#3421 = CARTESIAN_POINT ( 'NONE',  ( 20.00000000000000000, -5.510910596163090344E-15, 25.00000000000000000 ) ) ;
#3422 = VERTEX_POINT ( 'NONE', #7282 ) ;
#3423 = PLANE ( 'NONE',  #1845 ) ;
#3424 = CARTESIAN_POINT ( 'NONE',  ( 3.878096787214409868, 3.381939201670029149, 1.142309474598562469 ) ) ;
#3425 = EDGE_LOOP ( 'NONE', ( #9427, #1910 ) ) ;
#3426 = ORIENTED_EDGE ( 'NONE', *, *, #13922, .F. ) ;
#3427 = CARTESIAN_POINT ( 'NONE',  ( 0.000000000000000000, 40.49999999999999289, 8.000000000000007105 ) ) ;
#3428 = VERTEX_POINT ( 'NONE', #271 ) ;
#3429 = CARTESIAN_POINT ( 'NONE',  ( 4.158807179406251109, 2.089320655794530079, -3.499999999999992450 ) ) ;
#3430 = EDGE_CURVE ( 'NONE', #3225, #9041, #1920, .T. ) ;
#3431 = CARTESIAN_POINT ( 'NONE',  ( 59.10586122665984732, -20.42344490663941414, -35.00000000000000000 ) ) ;
#3432 = EDGE_CURVE ( 'NONE', #1577, #3032, #8227, .T. ) ;
#3433 = DIRECTION ( 'NONE',  ( -1.000000000000000000, 0.000000000000000000, 0.000000000000000000 ) ) ;
#3434 = CARTESIAN_POINT ( 'NONE',  ( -1.734723475976807094E-14, 35.49999999999996447, 0.000000000000000000 ) ) ;
#3435 = LINE ( 'NONE', #137, #13815 ) ;
#3436 = CARTESIAN_POINT ( 'NONE',  ( 6.726859516510133474, 4.293249649474419215E-15, -4.900000000000015454 ) ) ;
#3437 = CARTESIAN_POINT ( 'NONE',  ( 5.599999999999994316, -2.020725942163681399, 3.499999999999989342 ) ) ;
#3438 = CIRCLE ( 'NONE', #4149, 4.000000000000004441 ) ;
#3439 = CARTESIAN_POINT ( 'NONE',  ( 4.165266963751697915, -2.049631966911992453, 3.550066703508901966 ) ) ;
#3440 = ORIENTED_EDGE ( 'NONE', *, *, #4370, .T. ) ;
#3441 = ADVANCED_FACE ( 'NONE', ( #11529 ), #3714, .F. ) ;
#3442 = VERTEX_POINT ( 'NONE', #8378 ) ;
#3443 = ORIENTED_EDGE ( 'NONE', *, *, #13537, .F. ) ;
#3444 = CARTESIAN_POINT ( 'NONE',  ( -1.243833333691479526, 3.900674643483201365, -2.923144239647233356 ) ) ;
#3445 = ORIENTED_EDGE ( 'NONE', *, *, #5382, .F. ) ;
#3446 = ORIENTED_EDGE ( 'NONE', *, *, #2836, .T. ) ;
#3447 = DIRECTION ( 'NONE',  ( 0.000000000000000000, -0.4999999999999997224, 0.8660254037844387076 ) ) ;
#3448 = DIRECTION ( 'NONE',  ( -1.000000000000000000, 0.000000000000000000, 0.000000000000000000 ) ) ;
#3449 = CYLINDRICAL_SURFACE ( 'NONE', #6558, 13.00000000000002487 ) ;
#3450 = ORIENTED_EDGE ( 'NONE', *, *, #13375, .F. ) ;
#3451 = DIRECTION ( 'NONE',  ( 0.000000000000000000, 1.000000000000000000, 0.000000000000000000 ) ) ;
#3452 = DIRECTION ( 'NONE',  ( -8.138903065828892551E-32, 1.000000000000000000, 7.771561172376088880E-16 ) ) ;
#3453 = AXIS2_PLACEMENT_3D ( 'NONE', #9492, #3717, #7286 ) ;
#3454 = FILL_AREA_STYLE_COLOUR ( '', #12640 ) ;
#3455 = LINE ( 'NONE', #7900, #2154 ) ;
#3456 = ORIENTED_EDGE ( 'NONE', *, *, #3809, .T. ) ;
#3457 = PLANE ( 'NONE',  #3704 ) ;
#3458 = CARTESIAN_POINT ( 'NONE',  ( 3.370256023960729782E-15, 5.773502691896274186, -4.284345921091780696 ) ) ;
#3459 =( REPRESENTATION_RELATIONSHIP ('NONE','NONE', #10295, #2934 ) REPRESENTATION_RELATIONSHIP_WITH_TRANSFORMATION ( #200 )SHAPE_REPRESENTATION_RELATIONSHIP( ) );
#3460 = EDGE_CURVE ( 'NONE', #14384, #12535, #4736, .T. ) ;
#3461 = ORIENTED_EDGE ( 'NONE', *, *, #11129, .T. ) ;
#3462 = VECTOR ( 'NONE', #8588, 1000.000000000000114 ) ;
#3463 = VERTEX_POINT ( 'NONE', #1575 ) ;
#3464 = FACE_OUTER_BOUND ( 'NONE', #12416, .T. ) ;
#3465 = CARTESIAN_POINT ( 'NONE',  ( 22.00000000000000355, 30.00000000000000711, -25.00000000000000000 ) ) ;
#3466 = ADVANCED_FACE ( 'NONE', ( #6104 ), #8078, .F. ) ;
#3467 = LINE ( 'NONE', #7913, #13790 ) ;
#3468 = EDGE_CURVE ( 'NONE', #7396, #1865, #3793, .T. ) ;
#3469 = AXIS2_PLACEMENT_3D ( 'NONE', #11277, #8241, #7216 ) ;
#3470 = CARTESIAN_POINT ( 'NONE',  ( 5.046772446839278281, 2.317775331972814268, 4.014504635506723318 ) ) ;
#3471 = CIRCLE ( 'NONE', #7416, 4.999999999999976907 ) ;
#3472 = ORIENTED_EDGE ( 'NONE', *, *, #5559, .F. ) ;
#3473 = ORIENTED_EDGE ( 'NONE', *, *, #12175, .F. ) ;
#3474 = DIRECTION ( 'NONE',  ( 0.000000000000000000, 0.000000000000000000, 1.000000000000000000 ) ) ;
#3475 = ORIENTED_EDGE ( 'NONE', *, *, #620, .F. ) ;
#3476 = ADVANCED_FACE ( 'NONE', ( #3864, #3644 ), #3788, .F. ) ;
#3477 = PLANE ( 'NONE',  #11503 ) ;
#3478 = ADVANCED_FACE ( 'NONE', ( #10282 ), #342, .T. ) ;
#3479 = CONICAL_SURFACE ( 'NONE', #11642, 3.499999999999999112, 1.047197551196600296 ) ;
#3480 = ORIENTED_EDGE ( 'NONE', *, *, #7933, .F. ) ;
#3481 = VECTOR ( 'NONE', #11583, 1000.000000000000000 ) ;
#3482 = CARTESIAN_POINT ( 'NONE',  ( 20.00000000000000355, 40.00000000000000711, 25.00000000000000000 ) ) ;
#3483 = CARTESIAN_POINT ( 'NONE',  ( 0.000000000000000000, 0.000000000000000000, 4.750000000000000000 ) ) ;
#3484 = VECTOR ( 'NONE', #4651, 1000.000000000000000 ) ;
#3485 = CARTESIAN_POINT ( 'NONE',  ( 4.151274195509662590, -2.039912954708747339, -3.533232880573491830 ) ) ;
#3486 = DIRECTION ( 'NONE',  ( 6.608470384673545847E-17, -1.000000000000000000, 0.000000000000000000 ) ) ;
#3487 =( NAMED_UNIT ( * ) PLANE_ANGLE_UNIT ( ) SI_UNIT ( $, .RADIAN. ) );
#3488 = DIRECTION ( 'NONE',  ( -1.000000000000000000, 2.312964634635743943E-16, 0.000000000000000000 ) ) ;
#3489 = CARTESIAN_POINT ( 'NONE',  ( 20.00000000000000000, -5.510910596163090344E-15, -25.00000000000000000 ) ) ;
#3490 = ORIENTED_EDGE ( 'NONE', *, *, #5495, .F. ) ;
#3491 = DIRECTION ( 'NONE',  ( -1.000000000000000000, 0.000000000000000000, 0.000000000000000000 ) ) ;
#3492 = VERTEX_POINT ( 'NONE', #4872 ) ;
#3493 = DIRECTION ( 'NONE',  ( -1.000000000000000000, -1.913084959030911013E-15, -0.000000000000000000 ) ) ;
#3494 = AXIS2_PLACEMENT_3D ( 'NONE', #1742, #9568, #4014 ) ;
#3495 = CARTESIAN_POINT ( 'NONE',  ( 4.086376042167603195, 4.082715877136856797, -0.07147133206918650228 ) ) ;
#3496 = EDGE_CURVE ( 'NONE', #4363, #6994, #9478, .T. ) ;
#3497 = EDGE_LOOP ( 'NONE', ( #233, #6823, #1820, #10465 ) ) ;
#3498 = ORIENTED_EDGE ( 'NONE', *, *, #13558, .T. ) ;
#3499 = ORIENTED_EDGE ( 'NONE', *, *, #10742, .F. ) ;
#3500 = CARTESIAN_POINT ( 'NONE',  ( 24.99999999999998934, 189.5765550933606107, -2.000000000000001776 ) ) ;
#3501 = ORIENTED_EDGE ( 'NONE', *, *, #4235, .T. ) ;
#3502 = CARTESIAN_POINT ( 'NONE',  ( 68.68170757442801744, -83.66032599071898801, -106.9999999999999858 ) ) ;
#3503 = AXIS2_PLACEMENT_3D ( 'NONE', #4036, #7376, #10827 ) ;
#3504 = DIRECTION ( 'NONE',  ( -1.000000000000000000, 0.000000000000000000, 0.000000000000000000 ) ) ;
#3505 = CARTESIAN_POINT ( 'NONE',  ( 5.599999999999994316, 7.549649045036406812E-16, -2.499999999999999556 ) ) ;
#3506 = FACE_OUTER_BOUND ( 'NONE', #5037, .T. ) ;
#3507 = CARTESIAN_POINT ( 'NONE',  ( -108.6817075744280316, -30.42344490663958112, -32.00000000000002842 ) ) ;
#3508 = VECTOR ( 'NONE', #6555, 1000.000000000000000 ) ;
#3509 = CONTEXT_DEPENDENT_SHAPE_REPRESENTATION ( #2711, #9414 ) ;
#3510 = DIRECTION ( 'NONE',  ( 0.000000000000000000, 0.000000000000000000, -1.000000000000000000 ) ) ;
#3511 = CARTESIAN_POINT ( 'NONE',  ( 4.898587196589412829E-16, 17.49899999999995970, 3.469446951953614189E-15 ) ) ;
#3512 = VECTOR ( 'NONE', #12965, 1000.000000000000000 ) ;
#3513 = EDGE_CURVE ( 'NONE', #7122, #2216, #7020, .T. ) ;
#3514 = EDGE_LOOP ( 'NONE', ( #4060, #13471, #10647, #12366 ) ) ;
#3515 = CARTESIAN_POINT ( 'NONE',  ( -3.455075492487776234, 2.624013387858708413, -3.016622336521908920 ) ) ;
#3516 = ORIENTED_EDGE ( 'NONE', *, *, #4793, .T. ) ;
#3517 = ORIENTED_EDGE ( 'NONE', *, *, #6273, .T. ) ;
#3518 = CARTESIAN_POINT ( 'NONE',  ( 71.80728622811317052, -17.99808865627607801, 25.00000000000000000 ) ) ;
#3519 =( NAMED_UNIT ( * ) SI_UNIT ( $, .STERADIAN. ) SOLID_ANGLE_UNIT ( ) );
#3520 = CARTESIAN_POINT ( 'NONE',  ( 20.00000000000000000, -5.510910596163090344E-15, -25.00000000000000000 ) ) ;
#3521 = ORIENTED_EDGE ( 'NONE', *, *, #9684, .T. ) ;
#3522 = AXIS2_PLACEMENT_3D ( 'NONE', #10871, #5091, #6403 ) ;
#3523 = DIRECTION ( 'NONE',  ( 0.000000000000000000, 0.000000000000000000, -1.000000000000000000 ) ) ;
#3524 = DIRECTION ( 'NONE',  ( -4.664070103548418288E-16, -0.9242245927363028635, -0.3818493186865930533 ) ) ;
#3525 = EDGE_CURVE ( 'NONE', #6549, #7848, #2872, .T. ) ;
#3526 = LINE ( 'NONE', #7966, #14072 ) ;
#3527 = EDGE_LOOP ( 'NONE', ( #7676, #8823, #7369, #8131 ) ) ;
#3528 = ORIENTED_EDGE ( 'NONE', *, *, #6801, .T. ) ;
#3529 = CARTESIAN_POINT ( 'NONE',  ( 0.000000000000000000, -0.8660254037844428154, 1.500000000000001332 ) ) ;
#3530 = EDGE_CURVE ( 'NONE', #1693, #14098, #3551, .T. ) ;
#3531 = VECTOR ( 'NONE', #2273, 1000.000000000000000 ) ;
#3532 =( GEOMETRIC_REPRESENTATION_CONTEXT ( 3 ) GLOBAL_UNCERTAINTY_ASSIGNED_CONTEXT ( ( #9683 ) ) GLOBAL_UNIT_ASSIGNED_CONTEXT ( ( #4317, #8960, #7790 ) ) REPRESENTATION_CONTEXT ( 'NONE', 'WORKASPACE' ) );
#3533 = VECTOR ( 'NONE', #10987, 1000.000000000000000 ) ;
#3534 = ORIENTED_EDGE ( 'NONE', *, *, #13005, .T. ) ;
#3535 = AXIS2_PLACEMENT_3D ( 'NONE', #11507, #5932, #7175 ) ;
#3536 = FACE_OUTER_BOUND ( 'NONE', #9217, .T. ) ;
#3537 = CYLINDRICAL_SURFACE ( 'NONE', #11716, 2.749999999999997780 ) ;
#3538 = AXIS2_PLACEMENT_3D ( 'NONE', #3812, #14322, #11695 ) ;
#3539 = B_SPLINE_CURVE_WITH_KNOTS ( 'NONE', 3,
 ( #4796, #8144, #11971, #5234, #11900, #7194, #6181, #10653 ),
 .UNSPECIFIED., .F., .F.,
 ( 4, 2, 2, 4 ),
 ( 0.000000000000000000, 0.002450665683189818828, 0.003675998524784728459, 0.004901331366379637657 ),
 .UNSPECIFIED. ) ;
#3540 = PRESENTATION_STYLE_ASSIGNMENT (( #3405 ) ) ;
#3541 = ADVANCED_FACE ( 'NONE', ( #1737 ), #9841, .T. ) ;
#3542 = VECTOR ( 'NONE', #3817, 1000.000000000000000 ) ;
#3543 = VERTEX_POINT ( 'NONE', #14179 ) ;
#3544 = TOROIDAL_SURFACE ( 'NONE', #4005, 2.699999999999999289, 0.2000000000000000111 ) ;
#3545 = ORIENTED_EDGE ( 'NONE', *, *, #1555, .T. ) ;
#3546 = FACE_OUTER_BOUND ( 'NONE', #1076, .T. ) ;
#3547 = VECTOR ( 'NONE', #12816, 1000.000000000000000 ) ;
#3548 = CARTESIAN_POINT ( 'NONE',  ( 5.103021810857248042, 2.353405741491033876, -4.076218315086673982 ) ) ;
#3549 = ORIENTED_EDGE ( 'NONE', *, *, #9120, .T. ) ;
#3550 = EDGE_CURVE ( 'NONE', #6673, #79, #3338, .T. ) ;
#3551 = B_SPLINE_CURVE_WITH_KNOTS ( 'NONE', 3,
 ( #4803, #10508, #12855, #5877, #10363, #12619, #13741, #1511, #5953, #2988, #13224, #1805, #13015, #10935, #9563, #5167, #13159, #7486, #14113, #5304, #14041, #4008, #8595, #5240, #840, #8456, #9705, #5375, #8671, #9767, #7419, #4308, #4097, #6400 ),
 .UNSPECIFIED., .F., .F.,
 ( 4, 2, 2, 2, 2, 2, 2, 2, 2, 2, 2, 2, 2, 2, 2, 2, 4 ),
 ( 0.000000000000000000, 0.0007952457144059360810, 0.001590491428811872162, 0.002385737143217809327, 0.003180982857623746492, 0.003976228572029682357, 0.004771474286435620389, 0.005566720000841557554, 0.006361965715247495587, 0.007157211429653434487, 0.007952457144059371652, 0.008747702858465312287, 0.009542948572871249452, 0.01033819428727718835, 0.01113344000168312725, 0.01192868571608906615, 0.01272393143049500505 ),
 .UNSPECIFIED. ) ;
#3552 = DIRECTION ( 'NONE',  ( 1.000000000000000000, 0.000000000000000000, -0.000000000000000000 ) ) ;
#3553 = AXIS2_PLACEMENT_3D ( 'NONE', #13464, #2112, #68 ) ;
#3554 = UNCERTAINTY_MEASURE_WITH_UNIT (LENGTH_MEASURE( 1.000000000000000082E-05 ), #6295, 'distance_accuracy_value', 'NONE');
#3555 = STYLED_ITEM ( 'NONE', ( #9810 ), #13802 ) ;
#3556 = AXIS2_PLACEMENT_3D ( 'NONE', #8487, #12973, #4041 ) ;
#3557 = DIRECTION ( 'NONE',  ( 0.000000000000000000, 0.000000000000000000, -1.000000000000000000 ) ) ;
#3558 = DIRECTION ( 'NONE',  ( 0.000000000000000000, 0.000000000000000000, -1.000000000000000000 ) ) ;
#3559 = FACE_OUTER_BOUND ( 'NONE', #406, .T. ) ;
#3560 = DIRECTION ( 'NONE',  ( -0.2425356250363327748, 0.9701425001453319874, 0.000000000000000000 ) ) ;
#3561 = CARTESIAN_POINT ( 'NONE',  ( 71.80728622811317052, -17.99808865627607801, 25.00000000000000000 ) ) ;
#3562 = EDGE_CURVE ( 'NONE', #12012, #5916, #11978, .T. ) ;
#3563 = DIRECTION ( 'NONE',  ( 1.000000000000000000, 0.000000000000000000, -0.000000000000000000 ) ) ;
#3564 = VERTEX_POINT ( 'NONE', #6459 ) ;
#3565 = EDGE_CURVE ( 'NONE', #11502, #1577, #3196, .T. ) ;
#3566 = CARTESIAN_POINT ( 'NONE',  ( 68.68170757442801744, 39.57655509336063915, 33.00000000000002842 ) ) ;
#3567 = ORIENTED_EDGE ( 'NONE', *, *, #10690, .T. ) ;
#3568 = DIRECTION ( 'NONE',  ( -0.000000000000000000, 1.000000000000000000, -0.000000000000000000 ) ) ;
#3569 = AXIS2_PLACEMENT_3D ( 'NONE', #7986, #10479, #4841 ) ;
#3570 = VECTOR ( 'NONE', #2076, 1000.000000000000000 ) ;
#3571 = EDGE_LOOP ( 'NONE', ( #14354, #5002 ) ) ;
#3572 = CARTESIAN_POINT ( 'NONE',  ( 4.767554269344628004, -3.864655694377453266, -1.306219983577875832 ) ) ;
#3573 = VERTEX_POINT ( 'NONE', #14319 ) ;
#3574 = CARTESIAN_POINT ( 'NONE',  ( 0.000000000000000000, 0.000000000000000000, 0.000000000000000000 ) ) ;
#3575 = ORIENTED_EDGE ( 'NONE', *, *, #4447, .T. ) ;
#3576 = FACE_OUTER_BOUND ( 'NONE', #12792, .T. ) ;
#3577 = CIRCLE ( 'NONE', #4514, 4.999999999999988454 ) ;
#3578 = AXIS2_PLACEMENT_3D ( 'NONE', #8710, #1165, #6574 ) ;
#3579 = PRODUCT ( 'Wedge Roller Guide Pins', 'Wedge Roller Guide Pins', '', ( #14066 ) ) ;
#3580 = LINE ( 'NONE', #13461, #2750 ) ;
#3581 = EDGE_CURVE ( 'NONE', #1352, #1753, #6581, .T. ) ;
#3582 = DIRECTION ( 'NONE',  ( 0.000000000000000000, -0.000000000000000000, 1.000000000000000000 ) ) ;
#3583 = EDGE_CURVE ( 'NONE', #4300, #2949, #13082, .T. ) ;
#3584 = LINE ( 'NONE', #9339, #7245 ) ;
#3585 = DIRECTION ( 'NONE',  ( 0.000000000000000000, 1.000000000000000000, 0.000000000000000000 ) ) ;
#3586 = CARTESIAN_POINT ( 'NONE',  ( 5.103531824934115946, -2.354098498486438373, 4.077418205400141105 ) ) ;
#3587 = CYLINDRICAL_SURFACE ( 'NONE', #2385, 2.500000000000000444 ) ;
#3588 = AXIS2_PLACEMENT_3D ( 'NONE', #8981, #5408, #12220 ) ;
#3589 = EDGE_LOOP ( 'NONE', ( #5438, #11676, #5797, #921 ) ) ;
#3590 = ORIENTED_EDGE ( 'NONE', *, *, #13601, .T. ) ;
#3591 = FACE_OUTER_BOUND ( 'NONE', #9575, .T. ) ;
#3592 = VERTEX_POINT ( 'NONE', #644 ) ;
#3593 = ORIENTED_EDGE ( 'NONE', *, *, #12373, .F. ) ;
#3594 = LINE ( 'NONE', #13692, #922 ) ;
#3595 = CARTESIAN_POINT ( 'NONE',  ( 4.872112557122744825, -2.415761400130177830E-11, -4.072377784234180176 ) ) ;
#3596 = CARTESIAN_POINT ( 'NONE',  ( 88.22284556172391490, 29.57655509336062849, -106.9999999999999858 ) ) ;
#3597 = LINE ( 'NONE', #10235, #4268 ) ;
#3598 = CIRCLE ( 'NONE', #1245, 6.250000000000007105 ) ;
#3599 = EDGE_CURVE ( 'NONE', #12012, #3255, #7562, .T. ) ;
#3600 = DIRECTION ( 'NONE',  ( 1.000000000000000000, 1.665334536937734318E-16, 0.000000000000000000 ) ) ;
#3601 = EDGE_CURVE ( 'NONE', #619, #13436, #9629, .T. ) ;
#3602 = DIRECTION ( 'NONE',  ( 0.000000000000000000, 0.000000000000000000, 1.000000000000000000 ) ) ;
#3603 = DIRECTION ( 'NONE',  ( -2.243905293393255080E-15, 8.975621173573017164E-15, -1.000000000000000000 ) ) ;
#3604 = AXIS2_PLACEMENT_3D ( 'NONE', #1100, #4623, #12372 ) ;
#3605 = ORIENTED_EDGE ( 'NONE', *, *, #3650, .T. ) ;
#3606 = EDGE_CURVE ( 'NONE', #5482, #9930, #10659, .T. ) ;
#3607 = AXIS2_PLACEMENT_3D ( 'NONE', #5651, #113, #9088 ) ;
#3608 = DIRECTION ( 'NONE',  ( -0.2425356250363327748, 0.9701425001453319874, 0.000000000000000000 ) ) ;
#3609 = CARTESIAN_POINT ( 'NONE',  ( 129.3408537872138595, 189.5765550933606107, -4.000000000000019540 ) ) ;
#3610 =( NAMED_UNIT ( * ) PLANE_ANGLE_UNIT ( ) SI_UNIT ( $, .RADIAN. ) );
#3611 = EDGE_CURVE ( 'NONE', #8333, #11237, #7170, .T. ) ;
#3612 = DIRECTION ( 'NONE',  ( -1.000000000000000000, 1.892425610156516875E-16, 0.000000000000000000 ) ) ;
#3613 = EDGE_CURVE ( 'NONE', #7164, #4025, #174, .T. ) ;
#3614 = ORIENTED_EDGE ( 'NONE', *, *, #11485, .T. ) ;
#3615 = ORIENTED_EDGE ( 'NONE', *, *, #8571, .F. ) ;
#3616 = DIRECTION ( 'NONE',  ( -0.000000000000000000, 1.000000000000000000, -0.000000000000000000 ) ) ;
#3617 = CARTESIAN_POINT ( 'NONE',  ( 5.067058822021063058, 2.325541950156893911, -4.027956812804547759 ) ) ;
#3618 = ORIENTED_EDGE ( 'NONE', *, *, #3197, .F. ) ;
#3619 = EDGE_CURVE ( 'NONE', #4830, #337, #12114, .T. ) ;
#3620 = DIRECTION ( 'NONE',  ( -0.7071067811865467956, 0.7071067811865483499, 0.000000000000000000 ) ) ;
#3621 = EDGE_CURVE ( 'NONE', #7201, #7974, #3415, .T. ) ;
#3622 = EDGE_CURVE ( 'NONE', #6997, #10870, #2089, .T. ) ;
#3623 = CYLINDRICAL_SURFACE ( 'NONE', #9197, 9.000000000000001776 ) ;
#3624 = CARTESIAN_POINT ( 'NONE',  ( 4.158413352280787123, 2.044871626972824430, 3.541821552872956413 ) ) ;
#3625 = VERTEX_POINT ( 'NONE', #12185 ) ;
#3626 = CYLINDRICAL_SURFACE ( 'NONE', #237, 3.299999999999976730 ) ;
#3627 = CARTESIAN_POINT ( 'NONE',  ( 76.68170757442796059, 3.003422806631532356E-13, -199.4258611313499330 ) ) ;
#3628 = CARTESIAN_POINT ( 'NONE',  ( 108.6817075744280174, 109.5765550933605113, -3.299999999999986500 ) ) ;
#3629 = APPLICATION_CONTEXT ( 'automotive_design' ) ;
#3630 = CARTESIAN_POINT ( 'NONE',  ( 3.972709601346604114, 2.746729940827179028, -2.374099244652740914 ) ) ;
#3631 = CARTESIAN_POINT ( 'NONE',  ( 5.599999999999994316, 2.020725942163681399, 3.499999999999996003 ) ) ;
#3632 = ORIENTED_EDGE ( 'NONE', *, *, #9916, .F. ) ;
#3633 = FACE_OUTER_BOUND ( 'NONE', #6702, .T. ) ;
#3634 = DIRECTION ( 'NONE',  ( 0.000000000000000000, 0.000000000000000000, 1.000000000000000000 ) ) ;
#3635 = ORIENTED_EDGE ( 'NONE', *, *, #8949, .T. ) ;
#3636 = CARTESIAN_POINT ( 'NONE',  ( 5.005210273051230452, -2.263846804438352844, -4.078902314160335330 ) ) ;
#3637 = ORIENTED_EDGE ( 'NONE', *, *, #4763, .T. ) ;
#3638 = CIRCLE ( 'NONE', #12999, 300.0000000000001137 ) ;
#3639 = FACE_BOUND ( 'NONE', #10061, .T. ) ;
#3640 = VERTEX_POINT ( 'NONE', #14457 ) ;
#3641 = EDGE_CURVE ( 'NONE', #4271, #8264, #2319, .T. ) ;
#3642 = VERTEX_POINT ( 'NONE', #8877 ) ;
#3643 = CARTESIAN_POINT ( 'NONE',  ( 0.2486750293958585323, -1.933232340699151397, -4.000000000000002665 ) ) ;
#3644 = FACE_BOUND ( 'NONE', #8759, .T. ) ;
#3645 = ORIENTED_EDGE ( 'NONE', *, *, #12264, .F. ) ;
#3646 = LINE ( 'NONE', #4737, #12617 ) ;
#3647 = CARTESIAN_POINT ( 'NONE',  ( 5.000000000000001776, 3.131513003882766988, -4.327950126012554577 ) ) ;
#3648 = LINE ( 'NONE', #1436, #6034 ) ;
#3649 = CYLINDRICAL_SURFACE ( 'NONE', #12102, 4.000000000000000000 ) ;
#3650 = EDGE_CURVE ( 'NONE', #4944, #11701, #5582, .T. ) ;
#3651 = ITEM_DEFINED_TRANSFORMATION ( 'NONE', 'NONE', #14133,  #11025 ) ;
#3652 = CARTESIAN_POINT ( 'NONE',  ( 0.8144415599836820618, -5.303284638000498319, -0.2680587191991398166 ) ) ;
#3653 = LINE ( 'NONE', #4747, #12563 ) ;
#3654 = LINE ( 'NONE', #2619, #9149 ) ;
#3655 = EDGE_CURVE ( 'NONE', #4481, #7467, #6833, .T. ) ;
#3656 = PRODUCT_DEFINITION ( 'UNKNOWN', '', #8021, #10108 ) ;
#3657 = EDGE_CURVE ( 'NONE', #5508, #3642, #39, .T. ) ;
#3658 = ORIENTED_EDGE ( 'NONE', *, *, #11582, .F. ) ;
#3659 = CARTESIAN_POINT ( 'NONE',  ( 4.175813232069169878, -2.061359961916364725, 3.570380186727409200 ) ) ;
#3660 = ORIENTED_EDGE ( 'NONE', *, *, #11848, .F. ) ;
#3661 = ORIENTED_EDGE ( 'NONE', *, *, #4029, .T. ) ;
#3662 = LINE ( 'NONE', #8098, #8406 ) ;
#3663 = CARTESIAN_POINT ( 'NONE',  ( 5.000000000000003553, 2.886751345948121106, -4.369522543421430427 ) ) ;
#3664 = SURFACE_SIDE_STYLE ('',( #13695 ) ) ;
#3665 = LINE ( 'NONE', #5903, #12422 ) ;
#3666 = LINE ( 'NONE', #12510, #4702 ) ;
#3667 = DIRECTION ( 'NONE',  ( -1.000000000000000000, -5.046468293750711996E-16, -1.680811587828860421E-31 ) ) ;
#3668 = CARTESIAN_POINT ( 'NONE',  ( -5.560781378645534900, -2.450568166102175686E-16, -3.699999999999981082 ) ) ;
#3669 = VERTEX_POINT ( 'NONE', #11004 ) ;
#3670 = CARTESIAN_POINT ( 'NONE',  ( 37.35300976710104948, 100.8957249956400375, 25.00000000000000000 ) ) ;
#3671 = AXIS2_PLACEMENT_3D ( 'NONE', #14442, #5568, #10111 ) ;
#3672 = ORIENTED_EDGE ( 'NONE', *, *, #9342, .F. ) ;
#3673 = PRODUCT_DEFINITION_CONTEXT ( 'detailed design', #12047, 'design' ) ;
#3674 = ORIENTED_EDGE ( 'NONE', *, *, #8055, .F. ) ;
#3675 = CARTESIAN_POINT ( 'NONE',  ( -2.345747346278098888, 3.264484291692505202, -0.01223254789874009263 ) ) ;
#3676 = DIRECTION ( 'NONE',  ( 0.000000000000000000, 8.482162385747133845E-47, -1.000000000000000000 ) ) ;
#3677 = VECTOR ( 'NONE', #1474, 1000.000000000000000 ) ;
#3678 = ORIENTED_EDGE ( 'NONE', *, *, #7571, .F. ) ;
#3679 = ORIENTED_EDGE ( 'NONE', *, *, #10443, .T. ) ;
#3680 = DIRECTION ( 'NONE',  ( 1.000000000000000000, 0.000000000000000000, 0.000000000000000000 ) ) ;
#3681 = VECTOR ( 'NONE', #918, 1000.000000000000000 ) ;
#3682 = DIRECTION ( 'NONE',  ( -1.000000000000000000, 0.000000000000000000, 0.000000000000000000 ) ) ;
#3683 = VERTEX_POINT ( 'NONE', #5713 ) ;
#3684 = DIRECTION ( 'NONE',  ( 1.000000000000000000, 1.665334536937734071E-16, 0.000000000000000000 ) ) ;
#3685 = EDGE_CURVE ( 'NONE', #6397, #10504, #983, .T. ) ;
#3686 = EDGE_CURVE ( 'NONE', #3050, #8106, #8460, .T. ) ;
#3687 = UNCERTAINTY_MEASURE_WITH_UNIT (LENGTH_MEASURE( 1.000000000000000082E-05 ), #4854, 'distance_accuracy_value', 'NONE');
#3688 = CARTESIAN_POINT ( 'NONE',  ( 28.00000000000000355, 29.99999999999999645, -24.99999999999999289 ) ) ;
#3689 = DIRECTION ( 'NONE',  ( 0.7071067811865467956, -0.7071067811865483499, -0.000000000000000000 ) ) ;
#3690 = VECTOR ( 'NONE', #3143, 1000.000000000000000 ) ;
#3691 = AXIS2_PLACEMENT_3D ( 'NONE', #8624, #11032, #6635 ) ;
#3692 = CARTESIAN_POINT ( 'NONE',  ( -5.238715782502661789, 1.018209582082211906, -4.386015505371675616 ) ) ;
#3693 = CARTESIAN_POINT ( 'NONE',  ( -28.00000000000000355, 29.99999999999999645, 8.000000000000007105 ) ) ;
#3694 = DIRECTION ( 'NONE',  ( 0.000000000000000000, 1.000000000000000000, 0.000000000000000000 ) ) ;
#3695 = B_SPLINE_CURVE_WITH_KNOTS ( 'NONE', 3,
 ( #11378, #12487, #5670, #11451, #11240, #9105 ),
 .UNSPECIFIED., .F., .F.,
 ( 4, 2, 4 ),
 ( 0.000000000000000000, 0.002383230369971167488, 0.004766460739942334109 ),
 .UNSPECIFIED. ) ;
#3696 = CARTESIAN_POINT ( 'NONE',  ( -28.00000000000000355, 29.99999999999999645, 0.000000000000000000 ) ) ;
#3697 = VERTEX_POINT ( 'NONE', #11149 ) ;
#3698 = CARTESIAN_POINT ( 'NONE',  ( 22.00000000000000355, 47.00000000000000000, 25.00000000000000000 ) ) ;
#3699 = CARTESIAN_POINT ( 'NONE',  ( -3.081487911019577365E-30, 3.469446951953614189E-15, -6.000000000000005329 ) ) ;
#3700 = EDGE_CURVE ( 'NONE', #7329, #1352, #6685, .T. ) ;
#3701 = CARTESIAN_POINT ( 'NONE',  ( 4.851472949720938566, -4.233901974057253881, 0.6666666666666709595 ) ) ;
#3702 = EDGE_LOOP ( 'NONE', ( #4228, #12719 ) ) ;
#3703 = CARTESIAN_POINT ( 'NONE',  ( -3.000000000000000888, 3.836840991697820422E-15, -6.000000000000005329 ) ) ;
#3704 = AXIS2_PLACEMENT_3D ( 'NONE', #13832, #7831, #3804 ) ;
#3705 = DIRECTION ( 'NONE',  ( -1.000000000000000000, 0.000000000000000000, 0.000000000000000000 ) ) ;
#3706 = AXIS2_PLACEMENT_3D ( 'NONE', #9926, #3140, #3201 ) ;
#3708 = VERTEX_POINT ( 'NONE', #2237 ) ;
#3707 = EDGE_CURVE ( 'NONE', #2228, #8962, #5652, .T. ) ;
#3709 = CIRCLE ( 'NONE', #4194, 0.5671001622691687061 ) ;
#3710 = CARTESIAN_POINT ( 'NONE',  ( 5.046772446839293380, 4.635550663945619654, -3.696590807480215359E-18 ) ) ;
#3711 = VERTEX_POINT ( 'NONE', #4520 ) ;
#3712 = ORIENTED_EDGE ( 'NONE', *, *, #5383, .F. ) ;
#3713 = CARTESIAN_POINT ( 'NONE',  ( -3.999999999999996447, 2.309401076758494487, -3.133295621305376422 ) ) ;
#3714 = PLANE ( 'NONE',  #9634 ) ;
#3715 = ORIENTED_EDGE ( 'NONE', *, *, #2397, .T. ) ;
#3716 = CARTESIAN_POINT ( 'NONE',  ( 4.988724804725896966, -2.309401076758484272, 4.000000000000003553 ) ) ;
#3717 = DIRECTION ( 'NONE',  ( 1.000000000000000000, 2.133709875451472726E-16, 0.000000000000000000 ) ) ;
#3718 = CARTESIAN_POINT ( 'NONE',  ( 20.00000000000000355, 40.00000000000000711, 25.00000000000000000 ) ) ;
#3719 = FACE_BOUND ( 'NONE', #1538, .T. ) ;
#3720 =( GEOMETRIC_REPRESENTATION_CONTEXT ( 3 ) GLOBAL_UNCERTAINTY_ASSIGNED_CONTEXT ( ( #6001 ) ) GLOBAL_UNIT_ASSIGNED_CONTEXT ( ( #13961, #3939, #6335 ) ) REPRESENTATION_CONTEXT ( 'NONE', 'WORKASPACE' ) );
#3721 = CARTESIAN_POINT ( 'NONE',  ( 0.000000000000000000, 3.031088913245522320, 1.750000000000001554 ) ) ;
#3722 = LINE ( 'NONE', #6781, #7013 ) ;
#3723 = CARTESIAN_POINT ( 'NONE',  ( 2.100000000000000977, 3.497202527569243497E-16, 1.159999999999994369 ) ) ;
#3724 = EDGE_CURVE ( 'NONE', #6531, #2687, #7850, .T. ) ;
#3725 = LINE ( 'NONE', #7138, #8206 ) ;
#3726 = CARTESIAN_POINT ( 'NONE',  ( 0.000000000000000000, 0.000000000000000000, -4.699999999999981526 ) ) ;
#3727 = VERTEX_POINT ( 'NONE', #13293 ) ;
#3728 = FACE_OUTER_BOUND ( 'NONE', #8959, .T. ) ;
#3729 = VERTEX_POINT ( 'NONE', #2302 ) ;
#3730 = ORIENTED_EDGE ( 'NONE', *, *, #1749, .T. ) ;
#3731 = FACE_BOUND ( 'NONE', #1718, .T. ) ;
#3732 = VECTOR ( 'NONE', #8761, 1000.000000000000000 ) ;
#3733 = DIRECTION ( 'NONE',  ( 0.000000000000000000, 0.000000000000000000, 1.000000000000000000 ) ) ;
#3734 = CARTESIAN_POINT ( 'NONE',  ( 4.000000000000001776, 6.661338147750939243E-16, 13.31572692736082786 ) ) ;
#3735 =( REPRESENTATION_RELATIONSHIP ('NONE','NONE', #10295, #8802 ) REPRESENTATION_RELATIONSHIP_WITH_TRANSFORMATION ( #10082 )SHAPE_REPRESENTATION_RELATIONSHIP( ) );
#3736 = DIRECTION ( 'NONE',  ( 1.000000000000000000, 0.000000000000000000, 0.000000000000000000 ) ) ;
#3737 = DIRECTION ( 'NONE',  ( -1.000000000000000000, -1.723842398015259277E-15, 0.000000000000000000 ) ) ;
#3738 = DIRECTION ( 'NONE',  ( 1.000000000000000000, -2.551526159633733968E-19, -1.987661601597216239E-18 ) ) ;
#3739 = DIRECTION ( 'NONE',  ( 1.000000000000000000, 1.665334536937734071E-16, 0.000000000000000000 ) ) ;
#3740 = ADVANCED_FACE ( 'NONE', ( #10128 ), #114, .T. ) ;
#3741 = CARTESIAN_POINT ( 'NONE',  ( 1.655952806101424146, -3.662737355149054963, -1.706474927185875547E-14 ) ) ;
#3742 = B_SPLINE_CURVE_WITH_KNOTS ( 'NONE', 3,
 ( #11120, #6367, #6430, #12080, #7822, #10900, #7595, #5551 ),
 .UNSPECIFIED., .F., .F.,
 ( 4, 2, 2, 4 ),
 ( 0.007260997678543217211, 0.007995810154593266036, 0.008730622630643315729, 0.01020024758274341338 ),
 .UNSPECIFIED. ) ;
#3743 = EDGE_CURVE ( 'NONE', #11965, #11358, #1273, .T. ) ;
#3744 = DIRECTION ( 'NONE',  ( -0.000000000000000000, -0.000000000000000000, -1.000000000000000000 ) ) ;
#3745 = VECTOR ( 'NONE', #14215, 1000.000000000000000 ) ;
#3746 = ORIENTED_EDGE ( 'NONE', *, *, #429, .T. ) ;
#3747 = CARTESIAN_POINT ( 'NONE',  ( -1.532072935877364915E-15, -6.066067634115591467, -4.659491423763650886 ) ) ;
#3748 = DIRECTION ( 'NONE',  ( -1.000000000000000000, 0.000000000000000000, 0.000000000000000000 ) ) ;
#3749 = PRESENTATION_STYLE_ASSIGNMENT (( #611 ) ) ;
#3750 = ADVANCED_FACE ( 'NONE', ( #7708, #3845 ), #1490, .T. ) ;
#3751 = ORIENTED_EDGE ( 'NONE', *, *, #1371, .T. ) ;
#3752 = DIRECTION ( 'NONE',  ( 0.000000000000000000, 0.000000000000000000, 1.000000000000000000 ) ) ;
#3753 = CIRCLE ( 'NONE', #14053, 2.500000000000002220 ) ;
#3754 = PLANE ( 'NONE',  #11733 ) ;
#3755 = CONICAL_SURFACE ( 'NONE', #11940, 2.540000000000002700, 0.7853981633974502774 ) ;
#3756 = ORIENTED_EDGE ( 'NONE', *, *, #8491, .T. ) ;
#3757 = LINE ( 'NONE', #11573, #12946 ) ;
#3758 = ORIENTED_EDGE ( 'NONE', *, *, #9882, .F. ) ;
#3759 = CARTESIAN_POINT ( 'NONE',  ( -25.00000000000000000, -30.42444490663959300, 47.99999999999998579 ) ) ;
#3760 = CARTESIAN_POINT ( 'NONE',  ( 4.170895651974823259, 2.054890354522521001, 3.559174498016414834 ) ) ;
#3761 = CIRCLE ( 'NONE', #6546, 4.000000000000000000 ) ;
#3762 = DIRECTION ( 'NONE',  ( 0.000000000000000000, 0.000000000000000000, -1.000000000000000000 ) ) ;
#3763 = VECTOR ( 'NONE', #3918, 1000.000000000000000 ) ;
#3764 = LINE ( 'NONE', #9468, #2460 ) ;
#3765 = DIRECTION ( 'NONE',  ( -1.000000000000000000, -3.286707217423839940E-17, -2.273843122241288053E-18 ) ) ;
#3766 = DIRECTION ( 'NONE',  ( 1.000000000000000000, 0.000000000000000000, 0.000000000000000000 ) ) ;
#3767 = AXIS2_PLACEMENT_3D ( 'NONE', #3929, #7278, #11755 ) ;
#3768 = EDGE_LOOP ( 'NONE', ( #1891, #10744, #1509, #5493, #8172 ) ) ;
#3769 = EDGE_CURVE ( 'NONE', #2806, #9244, #12528, .T. ) ;
#3770 = DIRECTION ( 'NONE',  ( 0.000000000000000000, 0.000000000000000000, 1.000000000000000000 ) ) ;
#3771 = EDGE_CURVE ( 'NONE', #13637, #8706, #451, .T. ) ;
#3772 = ORIENTED_EDGE ( 'NONE', *, *, #14001, .F. ) ;
#3773 = CARTESIAN_POINT ( 'NONE',  ( 25.90000000000000213, 29.99999999999999645, -6.999999999999992006 ) ) ;
#3774 = CARTESIAN_POINT ( 'NONE',  ( 27.75000000000001066, 0.000000000000000000, 0.000000000000000000 ) ) ;
#3775 = ORIENTED_EDGE ( 'NONE', *, *, #3091, .F. ) ;
#3776 = CARTESIAN_POINT ( 'NONE',  ( 5.108705940669685752, -4.722350143107945541, 0.02431935820581593993 ) ) ;
#3777 = EDGE_CURVE ( 'NONE', #8106, #3050, #3828, .T. ) ;
#3778 = AXIS2_PLACEMENT_3D ( 'NONE', #4822, #3737, #2560 ) ;
#3779 = CARTESIAN_POINT ( 'NONE',  ( -140.0000000000003411, 199.5765550933606107, 47.99999999999998579 ) ) ;
#3780 = ORIENTED_EDGE ( 'NONE', *, *, #11568, .T. ) ;
#3781 =( GEOMETRIC_REPRESENTATION_CONTEXT ( 3 ) GLOBAL_UNCERTAINTY_ASSIGNED_CONTEXT ( ( #8647 ) ) GLOBAL_UNIT_ASSIGNED_CONTEXT ( ( #6065, #455, #534 ) ) REPRESENTATION_CONTEXT ( 'NONE', 'WORKASPACE' ) );
#3782 = AXIS2_PLACEMENT_3D ( 'NONE', #7673, #12447, #1102 ) ;
#3783 = ORIENTED_EDGE ( 'NONE', *, *, #2005, .F. ) ;
#3784 = CARTESIAN_POINT ( 'NONE',  ( -3.081487911019577365E-30, 3.469446951953614189E-15, -4.900000000000015454 ) ) ;
#3785 = ORIENTED_EDGE ( 'NONE', *, *, #9218, .T. ) ;
#3786 = ORIENTED_EDGE ( 'NONE', *, *, #11283, .F. ) ;
#3787 = DIRECTION ( 'NONE',  ( 0.000000000000000000, 0.000000000000000000, -1.000000000000000000 ) ) ;
#3788 = PLANE ( 'NONE',  #5864 ) ;
#3789 = ADVANCED_FACE ( 'NONE', ( #10486 ), #2585, .F. ) ;
#3790 = EDGE_LOOP ( 'NONE', ( #3853, #8591 ) ) ;
#3791 = CARTESIAN_POINT ( 'NONE',  ( 2.682243648011671588, 3.070208061305306213, -0.04852650426601810146 ) ) ;
#3792 = DIRECTION ( 'NONE',  ( 1.000000000000000000, 0.000000000000000000, 0.000000000000000000 ) ) ;
#3793 = CIRCLE ( 'NONE', #13617, 5.499999999999975131 ) ;
#3794 = CARTESIAN_POINT ( 'NONE',  ( 6.532899837730830939, 3.469446951953614189E-15, -6.000000000000005329 ) ) ;
#3795 = CARTESIAN_POINT ( 'NONE',  ( 3.961557105775776133, -1.423285172353590422, 3.499999999999993339 ) ) ;
#3796 = CIRCLE ( 'NONE', #8691, 3.299999999999983391 ) ;
#3797 = AXIS2_PLACEMENT_3D ( 'NONE', #3292, #6708, #4399 ) ;
#3798 = ORIENTED_EDGE ( 'NONE', *, *, #10446, .F. ) ;
#3799 = LINE ( 'NONE', #3507, #1396 ) ;
#3800 = EDGE_CURVE ( 'NONE', #12392, #11488, #4783, .T. ) ;
#3801 = CARTESIAN_POINT ( 'NONE',  ( 39.85300976710104948, 100.8957249956400375, -25.00000000000000000 ) ) ;
#3802 = CARTESIAN_POINT ( 'NONE',  ( -3.999999999999991562, 2.511479357205549157, -3.169254599242359305 ) ) ;
#3803 = CARTESIAN_POINT ( 'NONE',  ( -2.100000000000000089, -9.254442493598001840E-17, 1.159999999999994369 ) ) ;
#3804 = DIRECTION ( 'NONE',  ( 0.000000000000000000, -0.000000000000000000, -1.000000000000000000 ) ) ;
#3805 = VECTOR ( 'NONE', #8931, 1000.000000000000000 ) ;
#3806 = ORIENTED_EDGE ( 'NONE', *, *, #3298, .F. ) ;
#3807 = CARTESIAN_POINT ( 'NONE',  ( 4.898587196589412829E-16, 249.5765550933606391, 3.469446951953614189E-15 ) ) ;
#3808 = ORIENTED_EDGE ( 'NONE', *, *, #14296, .T. ) ;
#3809 = EDGE_CURVE ( 'NONE', #5579, #12256, #9706, .T. ) ;
#3810 = ORIENTED_EDGE ( 'NONE', *, *, #10855, .T. ) ;
#3811 = FACE_BOUND ( 'NONE', #12655, .T. ) ;
#3812 = CARTESIAN_POINT ( 'NONE',  ( 60.00000000000000000, -6.123233995736768255E-16, 25.00000000000000000 ) ) ;
#3813 = DIRECTION ( 'NONE',  ( -1.000000000000000000, 0.000000000000000000, 0.000000000000000000 ) ) ;
#3814 = FACE_OUTER_BOUND ( 'NONE', #9176, .T. ) ;
#3815 = DIRECTION ( 'NONE',  ( 0.000000000000000000, -5.551115123125782702E-17, -1.000000000000000000 ) ) ;
#3816 = ORIENTED_EDGE ( 'NONE', *, *, #3213, .T. ) ;
#3817 = DIRECTION ( 'NONE',  ( -1.000000000000000000, 0.000000000000000000, 0.000000000000000000 ) ) ;
#3818 = DIRECTION ( 'NONE',  ( 0.000000000000000000, 0.000000000000000000, -1.000000000000000000 ) ) ;
#3819 = FACE_OUTER_BOUND ( 'NONE', #6811, .T. ) ;
#3820 = STYLED_ITEM ( 'NONE', ( #6669 ), #13112 ) ;
#3821 = DIRECTION ( 'NONE',  ( 0.000000000000000000, 0.000000000000000000, 1.000000000000000000 ) ) ;
#3822 = CIRCLE ( 'NONE', #2406, 4.000000000000000000 ) ;
#3823 = PRODUCT_DEFINITION_SHAPE ( 'NONE', 'NONE',  #9731 ) ;
#3824 = DIRECTION ( 'NONE',  ( -0.9701425001453319874, -0.2425356250363330801, -0.000000000000000000 ) ) ;
#3825 = EDGE_LOOP ( 'NONE', ( #23, #12009, #7737, #4310 ) ) ;
#3826 = VERTEX_POINT ( 'NONE', #10408 ) ;
#3827 = APPLICATION_CONTEXT ( 'automotive_design' ) ;
#3828 = CIRCLE ( 'NONE', #10116, 2.500000000000002220 ) ;
#3829 = EDGE_CURVE ( 'NONE', #5807, #3708, #2737, .T. ) ;
#3830 = EDGE_LOOP ( 'NONE', ( #516, #1949 ) ) ;
#3831 = VECTOR ( 'NONE', #3620, 1000.000000000000000 ) ;
#3832 = DIRECTION ( 'NONE',  ( -2.273843122241270334E-18, -5.551115123125782702E-17, -1.000000000000000000 ) ) ;
#3833 = CARTESIAN_POINT ( 'NONE',  ( 4.175813232069169878, 2.061359961916364725, 3.570380186727388327 ) ) ;
#3834 = VECTOR ( 'NONE', #2186, 1000.000000000000000 ) ;
#3835 = VERTEX_POINT ( 'NONE', #7992 ) ;
#3836 = PRODUCT_DEFINITION_FORMATION_WITH_SPECIFIED_SOURCE ( 'ANY', '', #10587, .NOT_KNOWN. ) ;
#3837 = LINE ( 'NONE', #4997, #676 ) ;
#3838 = CARTESIAN_POINT ( 'NONE',  ( -5.211749180171794116, -2.764497899775275602, -4.327903350935043747 ) ) ;
#3839 = ORIENTED_EDGE ( 'NONE', *, *, #1363, .T. ) ;
#3840 = CARTESIAN_POINT ( 'NONE',  ( 0.000000000000000000, 0.000000000000000000, -4.699999999999981526 ) ) ;
#3841 = EDGE_LOOP ( 'NONE', ( #4223, #4838, #6224, #9368 ) ) ;
#3842 = EDGE_CURVE ( 'NONE', #3826, #992, #13871, .T. ) ;
#3843 = EDGE_CURVE ( 'NONE', #254, #13727, #10343, .T. ) ;
#3844 = CARTESIAN_POINT ( 'NONE',  ( 20.00000000000000355, 40.00000000000000711, 25.00000000000000000 ) ) ;
#3845 = FACE_BOUND ( 'NONE', #6428, .T. ) ;
#3846 = ORIENTED_EDGE ( 'NONE', *, *, #6197, .T. ) ;
#3847 = CARTESIAN_POINT ( 'NONE',  ( 4.142654963991842187, 4.070796997468695722, -7.041181996303254420E-15 ) ) ;
#3848 = DIRECTION ( 'NONE',  ( 0.000000000000000000, 0.000000000000000000, 1.000000000000000000 ) ) ;
#3849 =( NAMED_UNIT ( * ) SI_UNIT ( $, .STERADIAN. ) SOLID_ANGLE_UNIT ( ) );
#3850 = DIRECTION ( 'NONE',  ( 1.000000000000000000, 1.665334536937734071E-16, 0.000000000000000000 ) ) ;
#3851 = PLANE ( 'NONE',  #880 ) ;
#3852 = EDGE_CURVE ( 'NONE', #8822, #408, #5666, .T. ) ;
#3853 = ORIENTED_EDGE ( 'NONE', *, *, #11500, .T. ) ;
#3854 = FILL_AREA_STYLE_COLOUR ( '', #24 ) ;
#3855 = DIRECTION ( 'NONE',  ( 0.000000000000000000, 0.000000000000000000, 1.000000000000000000 ) ) ;
#3856 = DIRECTION ( 'NONE',  ( 0.000000000000000000, 0.000000000000000000, -1.000000000000000000 ) ) ;
#3857 = ORIENTED_EDGE ( 'NONE', *, *, #6417, .F. ) ;
#3858 = CARTESIAN_POINT ( 'NONE',  ( 4.862831555539507633, -2.651660758729945666, -3.407188841443101524 ) ) ;
#3859 = CARTESIAN_POINT ( 'NONE',  ( 5.108705940669691969, 4.722350143107947318, -0.02431935820580391483 ) ) ;
#3860 = CARTESIAN_POINT ( 'NONE',  ( 5.076540720129197659, 4.661016483905926044, -1.388525000602713847E-14 ) ) ;
#3861 = ORIENTED_EDGE ( 'NONE', *, *, #8889, .T. ) ;
#3862 = VERTEX_POINT ( 'NONE', #2667 ) ;
#3863 = DIRECTION ( 'NONE',  ( 2.133709875451472726E-16, -1.000000000000000000, -0.000000000000000000 ) ) ;
#3864 = FACE_OUTER_BOUND ( 'NONE', #10022, .T. ) ;
#3865 = SHAPE_REPRESENTATION ( 'socket button head screw_iso_ISO 7380 - M5 x 25 - 25N', ( #11025 ), #10079 ) ;
#3866 = DIRECTION ( 'NONE',  ( 0.000000000000000000, 0.000000000000000000, 1.000000000000000000 ) ) ;
#3867 = CARTESIAN_POINT ( 'NONE',  ( -129.3408537872145132, 199.5765550933606107, -80.00000000000001421 ) ) ;
#3868 = CARTESIAN_POINT ( 'NONE',  ( 20.00000000000000355, 30.00000000000000711, -25.00000000000000000 ) ) ;
#3869 = DIRECTION ( 'NONE',  ( 0.000000000000000000, 8.482162385747133845E-47, -1.000000000000000000 ) ) ;
#3870 = CARTESIAN_POINT ( 'NONE',  ( 118.6817075744280174, -20.42344490663938927, -117.0000000000000000 ) ) ;
#3871 = CARTESIAN_POINT ( 'NONE',  ( 4.872112557121027976, -0.7881298154075988549, 4.072377784234137543 ) ) ;
#3872 = FACE_OUTER_BOUND ( 'NONE', #8424, .T. ) ;
#3873 = CARTESIAN_POINT ( 'NONE',  ( -0.4012132626380665590, -5.541862106709760205, -0.4203182062997351531 ) ) ;
#3874 = EDGE_CURVE ( 'NONE', #12513, #2459, #11577, .T. ) ;
#3875 = ORIENTED_EDGE ( 'NONE', *, *, #6043, .T. ) ;
#3876 = EDGE_CURVE ( 'NONE', #7437, #8618, #1554, .T. ) ;
#3877 = LINE ( 'NONE', #1673, #5911 ) ;
#3878 = VERTEX_POINT ( 'NONE', #9388 ) ;
#3879 = ADVANCED_FACE ( 'NONE', ( #6895 ), #12916, .F. ) ;
#3880 = ORIENTED_EDGE ( 'NONE', *, *, #1415, .F. ) ;
#3881 = DIRECTION ( 'NONE',  ( 0.000000000000000000, 0.000000000000000000, 1.000000000000000000 ) ) ;
#3882 = CARTESIAN_POINT ( 'NONE',  ( -3.999999999999996447, 0.9868501483902497595, -0.09357334158579269645 ) ) ;
#3883 = DIRECTION ( 'NONE',  ( 0.000000000000000000, 0.000000000000000000, -1.000000000000000000 ) ) ;
#3884 = DIRECTION ( 'NONE',  ( 0.000000000000000000, 1.000000000000000000, 0.000000000000000000 ) ) ;
#3885 = CARTESIAN_POINT ( 'NONE',  ( 4.988724804725785944, -2.309401076758511806, -3.999999999999989786 ) ) ;
#3886 = CARTESIAN_POINT ( 'NONE',  ( 0.2175679805369626907, -1.691499766289308537, 3.499999999999996447 ) ) ;
#3887 = DIRECTION ( 'NONE',  ( 5.551115123125782702E-17, -2.775557561562891351E-17, 1.000000000000000000 ) ) ;
#3888 = LINE ( 'NONE', #8403, #8466 ) ;
#3889 = DIRECTION ( 'NONE',  ( 0.000000000000000000, 0.000000000000000000, -1.000000000000000000 ) ) ;
#3890 = EDGE_CURVE ( 'NONE', #1128, #11372, #12840, .T. ) ;
#3891 = CARTESIAN_POINT ( 'NONE',  ( 4.817183509279845843, 3.279805190042297536, -4.566911319714219708 ) ) ;
#3892 = ORIENTED_EDGE ( 'NONE', *, *, #13707, .T. ) ;
#3893 = VERTEX_POINT ( 'NONE', #13935 ) ;
#3894 = ORIENTED_EDGE ( 'NONE', *, *, #4568, .F. ) ;
#3895 = DIRECTION ( 'NONE',  ( 0.000000000000000000, -1.000000000000000000, 0.000000000000000000 ) ) ;
#3896 = LINE ( 'NONE', #12739, #12186 ) ;
#3897 = SHAPE_REPRESENTATION_RELATIONSHIP ( 'NONE' , 'NONE' ,  #2934, #2974 ) ;
#3898 = ORIENTED_EDGE ( 'NONE', *, *, #9778, .T. ) ;
#3899 = ORIENTED_EDGE ( 'NONE', *, *, #6661, .F. ) ;
#3900 = DIRECTION ( 'NONE',  ( -1.000000000000000000, 0.000000000000000000, 0.000000000000000000 ) ) ;
#3901 = EDGE_CURVE ( 'NONE', #4341, #6772, #14016, .T. ) ;
#3902 = CARTESIAN_POINT ( 'NONE',  ( -1.721886139900566270, -5.052888355618796901, -4.357689166958457427 ) ) ;
#3903 = AXIS2_PLACEMENT_3D ( 'NONE', #1713, #9687, #6235 ) ;
#3904 = EDGE_LOOP ( 'NONE', ( #12922, #13029, #8344, #1792 ) ) ;
#3905 = CARTESIAN_POINT ( 'NONE',  ( -5.029394918168160089, -2.903722509865338530, -4.451004066889660216 ) ) ;
#3906 = B_SPLINE_CURVE_WITH_KNOTS ( 'NONE', 3,
 ( #11304, #6616, #13585, #8062, #5586, #7855 ),
 .UNSPECIFIED., .F., .F.,
 ( 4, 2, 4 ),
 ( 0.000000000000000000, 0.0002095117440854745035, 0.0004190234881709490071 ),
 .UNSPECIFIED. ) ;
#3907 = CARTESIAN_POINT ( 'NONE',  ( 0.1597025669805195447, 1.557591170365174804, -4.000000000000004441 ) ) ;
#3908 = DIRECTION ( 'NONE',  ( -1.000000000000000000, 0.000000000000000000, 0.000000000000000000 ) ) ;
#3909 = DIRECTION ( 'NONE',  ( 0.000000000000000000, 0.000000000000000000, -1.000000000000000000 ) ) ;
#3910 = ORIENTED_EDGE ( 'NONE', *, *, #8113, .T. ) ;
#3911 = DIRECTION ( 'NONE',  ( -1.000000000000000000, 0.000000000000000000, 0.000000000000000000 ) ) ;
#3912 = FACE_OUTER_BOUND ( 'NONE', #190, .T. ) ;
#3913 = EDGE_LOOP ( 'NONE', ( #14433, #10649, #12146, #1878 ) ) ;
#3914 = CARTESIAN_POINT ( 'NONE',  ( 13.00000000000000533, 29.99999999999999289, 8.000000000000007105 ) ) ;
#3915 = LINE ( 'NONE', #13800, #12568 ) ;
#3916 = VECTOR ( 'NONE', #1215, 999.9999999999998863 ) ;
#3917 = VERTEX_POINT ( 'NONE', #4140 ) ;
#3918 = DIRECTION ( 'NONE',  ( -2.243905293393255080E-15, 8.975621173573017164E-15, -1.000000000000000000 ) ) ;
#3919 = VECTOR ( 'NONE', #5955, 1000.000000000000000 ) ;
#3920 = VERTEX_POINT ( 'NONE', #3042 ) ;
#3921 = CARTESIAN_POINT ( 'NONE',  ( -6.726859516510170778, 4.293249649474423948E-15, -4.900000000000015454 ) ) ;
#3922 = ADVANCED_FACE ( 'NONE', ( #2001 ), #4209, .T. ) ;
#3923 = EDGE_CURVE ( 'NONE', #12157, #3193, #1855, .T. ) ;
#3924 = LINE ( 'NONE', #2597, #2904 ) ;
#3925 = EDGE_LOOP ( 'NONE', ( #11519, #5194, #110, #856, #383 ) ) ;
#3926 = DIRECTION ( 'NONE',  ( -0.000000000000000000, -0.000000000000000000, -1.000000000000000000 ) ) ;
#3927 = CARTESIAN_POINT ( 'NONE',  ( 4.767554269344989493, 3.864655694377410189, 1.306219983577960209 ) ) ;
#3928 = AXIS2_PLACEMENT_3D ( 'NONE', #9908, #3474, #9305 ) ;
#3929 = CARTESIAN_POINT ( 'NONE',  ( 19.99999999999999645, 67.00000000000000000, 25.00000000000000000 ) ) ;
#3930 = AXIS2_PLACEMENT_3D ( 'NONE', #2468, #13531, #12423 ) ;
#3931 = ORIENTED_EDGE ( 'NONE', *, *, #2706, .F. ) ;
#3932 = B_SPLINE_CURVE_WITH_KNOTS ( 'NONE', 3,
 ( #6571, #12013, #1915, #8915 ),
 .UNSPECIFIED., .F., .F.,
 ( 4, 4 ),
 ( 0.000000000000000000, 0.002376763279741518631 ),
 .UNSPECIFIED. ) ;
#3933 = PLANE ( 'NONE',  #12255 ) ;
#3934 = CARTESIAN_POINT ( 'NONE',  ( -1.999999999999994005, -3.464101615137768597, -2.842992957459221426 ) ) ;
#3935 = ORIENTED_EDGE ( 'NONE', *, *, #10334, .T. ) ;
#3936 = CARTESIAN_POINT ( 'NONE',  ( 4.151274195509659926, -4.079825909417491125, -1.361623441637700086E-14 ) ) ;
#3937 = PRODUCT ( 'torque nut 04-2_iso_ISO 7043-M5-N', 'torque nut 04-2_iso_ISO 7043-M5-N', '', ( #11856 ) ) ;
#3938 = CARTESIAN_POINT ( 'NONE',  ( 5.551115123125782702E-14, -3.464101615137743728, 2.000000000000001776 ) ) ;
#3939 =( NAMED_UNIT ( * ) PLANE_ANGLE_UNIT ( ) SI_UNIT ( $, .RADIAN. ) );
#3940 = DIRECTION ( 'NONE',  ( 1.913084959030911013E-15, -1.000000000000000000, 0.000000000000000000 ) ) ;
#3941 = CARTESIAN_POINT ( 'NONE',  ( 3.000000000000001332, 4.996003610813205418E-16, 1.599999999999990319 ) ) ;
#3942 = VECTOR ( 'NONE', #9599, 1000.000000000000000 ) ;
#3943 = DIRECTION ( 'NONE',  ( -1.000000000000000000, 0.000000000000000000, -0.000000000000000000 ) ) ;
#3944 = VECTOR ( 'NONE', #11620, 1000.000000000000000 ) ;
#3945 = DIRECTION ( 'NONE',  ( 1.000000000000000000, 4.625929269271485914E-16, 0.000000000000000000 ) ) ;
#3946 = CIRCLE ( 'NONE', #10711, 2.100000000000000977 ) ;
#3947 = EDGE_CURVE ( 'NONE', #45, #6127, #6164, .T. ) ;
#3948 = DIRECTION ( 'NONE',  ( 1.000000000000000000, 0.000000000000000000, 0.000000000000000000 ) ) ;
#3949 = CIRCLE ( 'NONE', #14000, 2.500000000000002220 ) ;
#3950 = EDGE_LOOP ( 'NONE', ( #1847, #1853, #9279, #11449 ) ) ;
#3951 = PLANE ( 'NONE',  #4993 ) ;
#3952 = ORIENTED_EDGE ( 'NONE', *, *, #17, .T. ) ;
#3953 = ORIENTED_EDGE ( 'NONE', *, *, #7524, .T. ) ;
#3954 = AXIS2_PLACEMENT_3D ( 'NONE', #12297, #11332, #5619 ) ;
#3955 = CARTESIAN_POINT ( 'NONE',  ( 28.00000000000000355, 35.49999999999997868, 0.000000000000000000 ) ) ;
#3956 = CARTESIAN_POINT ( 'NONE',  ( -0.6448876103708461871, -4.246476118072359363, -0.2256878752776786956 ) ) ;
#3957 = LINE ( 'NONE', #2864, #3047 ) ;
#3958 = AXIS2_PLACEMENT_3D ( 'NONE', #7060, #13745, #10512 ) ;
#3959 = DIRECTION ( 'NONE',  ( 0.9240638205168503205, -0.3822382184081049572, -0.000000000000000000 ) ) ;
#3960 = CARTESIAN_POINT ( 'NONE',  ( 0.000000000000000000, -30.42444490663959300, -32.00000000000002842 ) ) ;
#3961 = CARTESIAN_POINT ( 'NONE',  ( 34.92765351673772045, 110.5971499970933536, 25.00000000000000000 ) ) ;
#3962 = CARTESIAN_POINT ( 'NONE',  ( -28.00000000000000355, 29.99999999999999645, -40.12500000000000000 ) ) ;
#3963 = DIRECTION ( 'NONE',  ( 0.000000000000000000, 0.000000000000000000, 1.000000000000000000 ) ) ;
#3964 = LINE ( 'NONE', #13111, #35 ) ;
#3965 = EDGE_CURVE ( 'NONE', #3170, #9934, #5143, .T. ) ;
#3966 = LINE ( 'NONE', #1835, #12449 ) ;
#3967 = ORIENTED_EDGE ( 'NONE', *, *, #72, .F. ) ;
#3968 = DIRECTION ( 'NONE',  ( 0.000000000000000000, 0.000000000000000000, -1.000000000000000000 ) ) ;
#3969 = CARTESIAN_POINT ( 'NONE',  ( 0.3126073911696169993, 2.020725942163681399, 3.499999999999996003 ) ) ;
#3970 = EDGE_CURVE ( 'NONE', #6982, #1393, #11344, .T. ) ;
#3971 = STYLED_ITEM ( 'NONE', ( #12209 ), #6767 ) ;
#3972 =( LENGTH_UNIT ( ) NAMED_UNIT ( * ) SI_UNIT ( .MILLI., .METRE. ) );
#3973 = ORIENTED_EDGE ( 'NONE', *, *, #2716, .T. ) ;
#3974 = STYLED_ITEM ( 'NONE', ( #13477 ), #1997 ) ;
#3975 = EDGE_CURVE ( 'NONE', #1103, #7272, #12644, .T. ) ;
#3976 = ORIENTED_EDGE ( 'NONE', *, *, #6320, .F. ) ;
#3977 = DIRECTION ( 'NONE',  ( 0.000000000000000000, -1.000000000000000000, 0.000000000000000000 ) ) ;
#3978 = CARTESIAN_POINT ( 'NONE',  ( 4.000000000000002665, 0.7924765000094613487, -0.05906175389890213484 ) ) ;
#3979 = ORIENTED_EDGE ( 'NONE', *, *, #11946, .F. ) ;
#3980 = LINE ( 'NONE', #9814, #13415 ) ;
#3981 = AXIS2_PLACEMENT_3D ( 'NONE', #8549, #9580, #3010 ) ;
#3982 = EDGE_LOOP ( 'NONE', ( #2204, #5798, #9755, #3615 ) ) ;
#3983 = UNCERTAINTY_MEASURE_WITH_UNIT (LENGTH_MEASURE( 1.000000000000000082E-05 ), #11535, 'distance_accuracy_value', 'NONE');
#3984 = CARTESIAN_POINT ( 'NONE',  ( -7.999999999999992895, 0.000000000000000000, -4.699999999999981526 ) ) ;
#3985 = DIRECTION ( 'NONE',  ( -0.9701425001453319874, -0.2425356250363330801, -0.000000000000000000 ) ) ;
#3986 = CARTESIAN_POINT ( 'NONE',  ( -28.00000000000000355, 29.99999999999999645, 8.000000000000007105 ) ) ;
#3987 = EDGE_LOOP ( 'NONE', ( #11996, #8439, #12869, #2493 ) ) ;
#3988 = EDGE_CURVE ( 'NONE', #1377, #11964, #7544, .T. ) ;
#3989 = LINE ( 'NONE', #766, #8413 ) ;
#3990 = DIRECTION ( 'NONE',  ( 1.000000000000000000, 1.224646799147353454E-16, 0.000000000000000000 ) ) ;
#3991 = VERTEX_POINT ( 'NONE', #1932 ) ;
#3992 = CARTESIAN_POINT ( 'NONE',  ( -28.00000000000000355, 29.99999999999999645, 8.000000000000007105 ) ) ;
#3993 = PLANE ( 'NONE',  #12653 ) ;
#3994 = ORIENTED_EDGE ( 'NONE', *, *, #1415, .T. ) ;
#3995 = AXIS2_PLACEMENT_3D ( 'NONE', #5176, #10738, #5250 ) ;
#3996 = VECTOR ( 'NONE', #8356, 1000.000000000000000 ) ;
#3997 = CARTESIAN_POINT ( 'NONE',  ( 2.285412292771018983, 4.454019289455643182, -8.322945739720751976E-15 ) ) ;
#3998 = CARTESIAN_POINT ( 'NONE',  ( 3.522881874163210636, -2.820349071480532377, -3.298443181295927840 ) ) ;
#3999 = EDGE_LOOP ( 'NONE', ( #5182, #7262, #9638, #5982 ) ) ;
#4000 = FACE_OUTER_BOUND ( 'NONE', #6541, .T. ) ;
#4001 = FACE_OUTER_BOUND ( 'NONE', #12740, .T. ) ;
#4002 = DIRECTION ( 'NONE',  ( 0.000000000000000000, 0.000000000000000000, -1.000000000000000000 ) ) ;
#4003 = ORIENTED_EDGE ( 'NONE', *, *, #4989, .T. ) ;
#4004 = AXIS2_PLACEMENT_3D ( 'NONE', #11254, #4810, #12558 ) ;
#4005 = AXIS2_PLACEMENT_3D ( 'NONE', #8064, #8215, #1209 ) ;
#4006 = ORIENTED_EDGE ( 'NONE', *, *, #4989, .F. ) ;
#4007 = CARTESIAN_POINT ( 'NONE',  ( 20.00000000000000000, 70.00000000000000000, 25.00000000000000000 ) ) ;
#4008 = CARTESIAN_POINT ( 'NONE',  ( -3.587774770580208550, 47.65128983029578080, 2.212041269487583950 ) ) ;
#4009 = ADVANCED_FACE ( 'NONE', ( #5218 ), #12030, .T. ) ;
#4010 = ORIENTED_EDGE ( 'NONE', *, *, #13678, .T. ) ;
#4011 = CARTESIAN_POINT ( 'NONE',  ( 4.055492966679334010, 3.795017426213870504, -0.5629142681435886919 ) ) ;
#4012 = CARTESIAN_POINT ( 'NONE',  ( 27.75000000000001066, 0.000000000000000000, 0.000000000000000000 ) ) ;
#4013 = ORIENTED_EDGE ( 'NONE', *, *, #4873, .T. ) ;
#4014 = DIRECTION ( 'NONE',  ( 0.2425356250363328581, -0.9701425001453318764, 0.000000000000000000 ) ) ;
#4015 = CIRCLE ( 'NONE', #11708, 2.749999999999997780 ) ;
#4016 = FACE_OUTER_BOUND ( 'NONE', #12106, .T. ) ;
#4017 = EDGE_LOOP ( 'NONE', ( #12721, #2901, #13639 ) ) ;
#4018 = CARTESIAN_POINT ( 'NONE',  ( 32.57694101601105530, 130.0000000000000000, -25.00000000000000000 ) ) ;
#4019 = AXIS2_PLACEMENT_3D ( 'NONE', #13769, #8321, #4759 ) ;
#4020 = COLOUR_RGB ( '', 0.31764706, 0.68627451, 0.89019608) ;
#4021 = AXIS2_PLACEMENT_3D ( 'NONE', #2947, #8699, #12005 ) ;
#4022 = FACE_OUTER_BOUND ( 'NONE', #12111, .T. ) ;
#4023 =( REPRESENTATION_RELATIONSHIP ('NONE','NONE', #10295, #4432 ) REPRESENTATION_RELATIONSHIP_WITH_TRANSFORMATION ( #11253 )SHAPE_REPRESENTATION_RELATIONSHIP( ) );
#4024 = AXIS2_PLACEMENT_3D ( 'NONE', #610, #2801, #7241 ) ;
#4025 = VERTEX_POINT ( 'NONE', #1786 ) ;
#4026 = ORIENTED_EDGE ( 'NONE', *, *, #6151, .F. ) ;
#4027 = CARTESIAN_POINT ( 'NONE',  ( 4.000000000000002665, 2.309401076758501592, -3.204271511726781707 ) ) ;
#4028 = AXIS2_PLACEMENT_3D ( 'NONE', #1081, #2261, #11252 ) ;
#4029 = EDGE_CURVE ( 'NONE', #5022, #8001, #5066, .T. ) ;
#4030 = ORIENTED_EDGE ( 'NONE', *, *, #11967, .F. ) ;
#4031 = CARTESIAN_POINT ( 'NONE',  ( 20.00000000000000355, 40.00000000000000711, -25.00000000000000000 ) ) ;
#4032 = STYLED_ITEM ( 'NONE', ( #3749 ), #10469 ) ;
#4033 = VECTOR ( 'NONE', #13846, 1000.000000000000000 ) ;
#4034 = EDGE_CURVE ( 'NONE', #12216, #7928, #13704, .T. ) ;
#4035 = LINE ( 'NONE', #439, #8633 ) ;
#4036 = CARTESIAN_POINT ( 'NONE',  ( 2.750000000000002665, 0.000000000000000000, 0.000000000000000000 ) ) ;
#4037 = CARTESIAN_POINT ( 'NONE',  ( 22.00000000000000000, 57.00000000000000000, -25.00000000000000000 ) ) ;
#4038 = FACE_OUTER_BOUND ( 'NONE', #6296, .T. ) ;
#4039 = SHAPE_DEFINITION_REPRESENTATION ( #8348, #5343 ) ;
#4040 = CARTESIAN_POINT ( 'NONE',  ( 31.44014396567294867, 21.68342561534834090, 8.000000000000007105 ) ) ;
#4041 = DIRECTION ( 'NONE',  ( -1.000000000000000000, 0.000000000000000000, 0.000000000000000000 ) ) ;
#4042 = ADVANCED_FACE ( 'NONE', ( #2965 ), #5357, .T. ) ;
#4043 = ORIENTED_EDGE ( 'NONE', *, *, #311, .F. ) ;
#4044 =( BOUNDED_SURFACE ( )  B_SPLINE_SURFACE ( 3, 2, ( 
 ( #2323, #9185, #1289 ),
 ( #4668, #7944, #9108 ),
 ( #13682, #2466, #11246 ),
 ( #10075, #4603, #13606 ),
 ( #9037, #6915, #11382 ),
 ( #3647, #13528, #274 ) ),
 .UNSPECIFIED., .F., .F., .F. ) 
 B_SPLINE_SURFACE_WITH_KNOTS ( ( 4, 2, 4 ),
 ( 3, 3 ),
 ( 0.02462021979145854675, 0.02768763742058376331, 0.03075505504970898335 ),
 ( 0.000000000000000000, 1.000000000000000000 ),
 .UNSPECIFIED. ) 
 GEOMETRIC_REPRESENTATION_ITEM ( )  RATIONAL_B_SPLINE_SURFACE ( (
 ( 1.000000000000000000, 0.8047781263388831263, 1.000000000000000000),
 ( 1.000000000000000000, 0.8123781044083938641, 1.000000000000000000),
 ( 1.000000000000000000, 0.8190664127994971011, 1.000000000000000000),
 ( 1.000000000000000000, 0.8192359367744610488, 1.000000000000000000),
 ( 1.000000000000000000, 0.8126133147547173197, 1.000000000000000000),
 ( 1.000000000000000000, 0.8047712418670134316, 1.000000000000000000) ) ) 
 REPRESENTATION_ITEM ( '' )  SURFACE ( )  );
#4045 = AXIS2_PLACEMENT_3D ( 'NONE', #14105, #5077, #11749 ) ;
#4046 = AXIS2_PLACEMENT_3D ( 'NONE', #10169, #1099, #9958 ) ;
#4047 = AXIS2_PLACEMENT_3D ( 'NONE', #22, #10114, #7082 ) ;
#4048 = DIRECTION ( 'NONE',  ( 0.000000000000000000, 0.000000000000000000, 1.000000000000000000 ) ) ;
#4049 = ORIENTED_EDGE ( 'NONE', *, *, #14434, .T. ) ;
#4050 = ORIENTED_EDGE ( 'NONE', *, *, #1611, .F. ) ;
#4051 = ORIENTED_EDGE ( 'NONE', *, *, #10125, .F. ) ;
#4052 = ADVANCED_FACE ( 'NONE', ( #2896 ), #6307, .F. ) ;
#4053 = EDGE_CURVE ( 'NONE', #12036, #131, #12295, .T. ) ;
#4054 = CARTESIAN_POINT ( 'NONE',  ( 58.68170757442803165, -86.08568224108226730, -28.00000000000000000 ) ) ;
#4055 = CARTESIAN_POINT ( 'NONE',  ( 3.973110223767151616, 2.262797354954571809E-11, 3.565797985667430225 ) ) ;
#4056 = CIRCLE ( 'NONE', #2173, 2.500000000000002220 ) ;
#4057 = AXIS2_PLACEMENT_3D ( 'NONE', #1842, #14074, #14147 ) ;
#4058 = SHAPE_REPRESENTATION_RELATIONSHIP ( 'NONE' , 'NONE' ,  #4961, #11496 ) ;
#4059 = EDGE_CURVE ( 'NONE', #7201, #11896, #10110, .T. ) ;
#4060 = ORIENTED_EDGE ( 'NONE', *, *, #11713, .T. ) ;
#4061 = DIRECTION ( 'NONE',  ( 0.000000000000000000, 0.000000000000000000, 1.000000000000000000 ) ) ;
#4062 = DIRECTION ( 'NONE',  ( 0.9240638205168505426, -0.3822382184081045131, -0.000000000000000000 ) ) ;
#4063 = ORIENTED_EDGE ( 'NONE', *, *, #6939, .T. ) ;
#4064 = EDGE_CURVE ( 'NONE', #2782, #663, #9970, .T. ) ;
#4065 = DIRECTION ( 'NONE',  ( 0.000000000000000000, 0.000000000000000000, -1.000000000000000000 ) ) ;
#4066 = ORIENTED_EDGE ( 'NONE', *, *, #1363, .F. ) ;
#4067 = CIRCLE ( 'NONE', #540, 3.000000000000000888 ) ;
#4068 = ORIENTED_EDGE ( 'NONE', *, *, #10686, .T. ) ;
#4069 = PRODUCT_DEFINITION_SHAPE ( 'NONE', 'NONE',  #14483 ) ;
#4070 = EDGE_CURVE ( 'NONE', #8001, #1525, #11284, .T. ) ;
#4071 = CARTESIAN_POINT ( 'NONE',  ( -5.184911785341500767, 2.993510214989689722, -4.630720594357042863 ) ) ;
#4072 = DIRECTION ( 'NONE',  ( 0.000000000000000000, 0.000000000000000000, 1.000000000000000000 ) ) ;
#4073 = CARTESIAN_POINT ( 'NONE',  ( 56.99999999999997868, -9.797174393178845379E-16, 25.00000000000000000 ) ) ;
#4074 = ADVANCED_FACE ( 'NONE', ( #2148 ), #3249, .F. ) ;
#4075 = VERTEX_POINT ( 'NONE', #4574 ) ;
#4076 = DIRECTION ( 'NONE',  ( 1.000000000000000000, 0.000000000000000000, 0.000000000000000000 ) ) ;
#4077 = FACE_BOUND ( 'NONE', #12479, .T. ) ;
#4078 = VERTEX_POINT ( 'NONE', #2224 ) ;
#4079 = CARTESIAN_POINT ( 'NONE',  ( 0.000000000000000000, 0.000000000000000000, 0.000000000000000000 ) ) ;
#4080 = AXIS2_PLACEMENT_3D ( 'NONE', #4206, #10845, #6158 ) ;
#4081 = ORIENTED_EDGE ( 'NONE', *, *, #3530, .T. ) ;
#4082 =( NAMED_UNIT ( * ) PLANE_ANGLE_UNIT ( ) SI_UNIT ( $, .RADIAN. ) );
#4083 = CARTESIAN_POINT ( 'NONE',  ( 22.00000000000000355, 30.00000000000000711, 25.00000000000000000 ) ) ;
#4084 = B_SPLINE_CURVE_WITH_KNOTS ( 'NONE', 3,
 ( #9748, #7335, #11955, #2818, #1856, #763 ),
 .UNSPECIFIED., .F., .F.,
 ( 4, 2, 4 ),
 ( 0.004317080428420414645, 0.005486165713042582756, 0.006655250997664750867 ),
 .UNSPECIFIED. ) ;
#4085 = FACE_OUTER_BOUND ( 'NONE', #2198, .T. ) ;
#4086 = AXIS2_PLACEMENT_3D ( 'NONE', #5968, #7071, #7140 ) ;
#4087 = ORIENTED_EDGE ( 'NONE', *, *, #2573, .T. ) ;
#4088 = DIRECTION ( 'NONE',  ( 0.000000000000000000, 0.000000000000000000, 1.000000000000000000 ) ) ;
#4089 = B_SPLINE_CURVE_WITH_KNOTS ( 'NONE', 3,
 ( #13754, #4570, #94, #4814, #9344 ),
 .UNSPECIFIED., .F., .F.,
 ( 4, 1, 4 ),
 ( 0.000000000000000000, 0.002309401076758504923, 0.004618802153517009845 ),
 .UNSPECIFIED. ) ;
#4090 = EDGE_CURVE ( 'NONE', #2107, #4685, #4812, .T. ) ;
#4091 = PLANE ( 'NONE',  #9661 ) ;
#4092 = VERTEX_POINT ( 'NONE', #10038 ) ;
#4093 = AXIS2_PLACEMENT_3D ( 'NONE', #5907, #369, #1462 ) ;
#4094 = ORIENTED_EDGE ( 'NONE', *, *, #1185, .T. ) ;
#4095 = ORIENTED_EDGE ( 'NONE', *, *, #5830, .F. ) ;
#4096 = CARTESIAN_POINT ( 'NONE',  ( 4.197393957002308440, -0.4069871074557449564, -3.203767560748910892 ) ) ;
#4097 = CARTESIAN_POINT ( 'NONE',  ( -0.2655919857739738044, 48.49999999999998579, 9.914050073752000185E-16 ) ) ;
#4098 = VERTEX_POINT ( 'NONE', #5432 ) ;
#4099 = CARTESIAN_POINT ( 'NONE',  ( 1.560000000000005826, 0.8660254037844428154, 1.500000000000001332 ) ) ;
#4100 = VECTOR ( 'NONE', #6698, 1000.000000000000000 ) ;
#4101 = DIRECTION ( 'NONE',  ( 0.000000000000000000, 0.000000000000000000, -1.000000000000000000 ) ) ;
#4102 = DIRECTION ( 'NONE',  ( 0.000000000000000000, 0.000000000000000000, -1.000000000000000000 ) ) ;
#4103 = CARTESIAN_POINT ( 'NONE',  ( 19.99999999999999645, 67.00000000000000000, 25.00000000000000000 ) ) ;
#4104 = VERTEX_POINT ( 'NONE', #8936 ) ;
#4105 =( NAMED_UNIT ( * ) PLANE_ANGLE_UNIT ( ) SI_UNIT ( $, .RADIAN. ) );
#4106 = PLANE ( 'NONE',  #176 ) ;
#4107 = CARTESIAN_POINT ( 'NONE',  ( 0.000000000000000000, 0.000000000000000000, 0.000000000000000000 ) ) ;
#4108 = EDGE_CURVE ( 'NONE', #1341, #2724, #14441, .T. ) ;
#4109 = ORIENTED_EDGE ( 'NONE', *, *, #7683, .T. ) ;
#4110 = ORIENTED_EDGE ( 'NONE', *, *, #9395, .T. ) ;
#4111 = ORIENTED_EDGE ( 'NONE', *, *, #10086, .F. ) ;
#4112 = DIRECTION ( 'NONE',  ( -0.2425356250363328026, 0.9701425001453319874, 0.000000000000000000 ) ) ;
#4113 = ORIENTED_EDGE ( 'NONE', *, *, #8262, .F. ) ;
#4114 = ORIENTED_EDGE ( 'NONE', *, *, #11328, .T. ) ;
#4115 = CYLINDRICAL_SURFACE ( 'NONE', #2813, 4.999999999999988454 ) ;
#4116 = CARTESIAN_POINT ( 'NONE',  ( 0.000000000000000000, 0.000000000000000000, 0.000000000000000000 ) ) ;
#4117 = CARTESIAN_POINT ( 'NONE',  ( 5.599999999999994316, 3.543787447695206106E-16, -5.200000000000001066 ) ) ;
#4118 = CARTESIAN_POINT ( 'NONE',  ( 0.000000000000000000, 25.49999999999996803, 0.000000000000000000 ) ) ;
#4119 = DIRECTION ( 'NONE',  ( 1.000000000000000000, 0.000000000000000000, 0.000000000000000000 ) ) ;
#4120 = PLANE ( 'NONE',  #4507 ) ;
#4121 = CARTESIAN_POINT ( 'NONE',  ( -28.00000000000000355, 29.99999999999999645, 8.000000000000007105 ) ) ;
#4122 = VERTEX_POINT ( 'NONE', #4290 ) ;
#4123 = EDGE_CURVE ( 'NONE', #7536, #12258, #10688, .T. ) ;
#4124 = ADVANCED_FACE ( 'NONE', ( #3464 ), #3400, .F. ) ;
#4125 = CARTESIAN_POINT ( 'NONE',  ( 3.667453972563985829E-15, 6.066067634115573703, -4.659491423763650886 ) ) ;
#4126 = VERTEX_POINT ( 'NONE', #7609 ) ;
#4127 = EDGE_LOOP ( 'NONE', ( #8029, #770, #8543, #2764 ) ) ;
#4128 = VERTEX_POINT ( 'NONE', #14373 ) ;
#4129 = CARTESIAN_POINT ( 'NONE',  ( 39.77836601746437850, 91.19429999418670718, -25.00000000000000000 ) ) ;
#4130 = DIRECTION ( 'NONE',  ( 1.224646799147353207E-16, 1.000000000000000000, 8.482162385747133845E-47 ) ) ;
#4131 = FILL_AREA_STYLE_COLOUR ( '', #3319 ) ;
#4132 = EDGE_LOOP ( 'NONE', ( #1146, #9603, #5796, #462 ) ) ;
#4133 = DIRECTION ( 'NONE',  ( 0.2425356250363327748, -0.9701425001453319874, -0.000000000000000000 ) ) ;
#4134 = AXIS2_PLACEMENT_3D ( 'NONE', #10706, #888, #4072 ) ;
#4135 = CARTESIAN_POINT ( 'NONE',  ( -4.319324222800883462, -3.279739689144915538, -4.138711833383139194 ) ) ;
#4136 = DIRECTION ( 'NONE',  ( 0.000000000000000000, 0.000000000000000000, -1.000000000000000000 ) ) ;
#4137 = ORIENTED_EDGE ( 'NONE', *, *, #4806, .F. ) ;
#4138 = UNCERTAINTY_MEASURE_WITH_UNIT (LENGTH_MEASURE( 1.000000000000000082E-05 ), #5511, 'distance_accuracy_value', 'NONE');
#4139 = CARTESIAN_POINT ( 'NONE',  ( 28.00000000000000355, 29.99999999999999645, -34.50000000000000000 ) ) ;
#4140 = CARTESIAN_POINT ( 'NONE',  ( 24.99999999999999289, 199.5765550933606107, -2.000000000000001776 ) ) ;
#4141 = LINE ( 'NONE', #1933, #3206 ) ;
#4142 = ORIENTED_EDGE ( 'NONE', *, *, #12817, .F. ) ;
#4143 = CARTESIAN_POINT ( 'NONE',  ( 4.158413352280787123, 4.089743253945648860, -1.387778780781445676E-14 ) ) ;
#4144 = CARTESIAN_POINT ( 'NONE',  ( 4.769954020850214249, 0.8342959359879871251, -4.000000000000002665 ) ) ;
#4145 = EDGE_LOOP ( 'NONE', ( #6323, #11922 ) ) ;
#4146 = DIRECTION ( 'NONE',  ( -1.000000000000000000, 0.000000000000000000, 0.000000000000000000 ) ) ;
#4147 = VERTEX_POINT ( 'NONE', #7910 ) ;
#4148 = SURFACE_STYLE_USAGE ( .BOTH. , #11585 ) ;
#4149 = AXIS2_PLACEMENT_3D ( 'NONE', #7825, #8780, #5626 ) ;
#4150 = CARTESIAN_POINT ( 'NONE',  ( 22.00000000000000711, 17.00000000000000000, 25.00000000000000000 ) ) ;
#4151 = CARTESIAN_POINT ( 'NONE',  ( 4.851472949721052252, -2.694301256218235796, 3.333333333333339699 ) ) ;
#4152 = EDGE_CURVE ( 'NONE', #13612, #1573, #12094, .T. ) ;
#4153 = VERTEX_POINT ( 'NONE', #1046 ) ;
#4154 = DIRECTION ( 'NONE',  ( 1.000000000000000000, 0.000000000000000000, 0.000000000000000000 ) ) ;
#4155 = DIRECTION ( 'NONE',  ( 0.000000000000000000, 0.000000000000000000, -1.000000000000000000 ) ) ;
#4156 = ORIENTED_EDGE ( 'NONE', *, *, #11847, .T. ) ;
#4157 = ORIENTED_EDGE ( 'NONE', *, *, #4348, .F. ) ;
#4158 = ORIENTED_EDGE ( 'NONE', *, *, #12918, .T. ) ;
#4159 = LINE ( 'NONE', #9704, #8506 ) ;
#4160 = DIRECTION ( 'NONE',  ( 1.000000000000000000, 0.000000000000000000, 0.000000000000000000 ) ) ;
#4161 = ORIENTED_EDGE ( 'NONE', *, *, #5552, .T. ) ;
#4162 = CARTESIAN_POINT ( 'NONE',  ( 5.046772446839306703, -2.317775331972796504, 4.014504635506726871 ) ) ;
#4163 = CARTESIAN_POINT ( 'NONE',  ( 60.00000000000000000, -6.123233995736768255E-16, 25.00000000000000000 ) ) ;
#4164 = CARTESIAN_POINT ( 'NONE',  ( 108.6817075744280743, 124.5765550933606107, -25.00000000000000000 ) ) ;
#4165 = EDGE_CURVE ( 'NONE', #2504, #10603, #8093, .T. ) ;
#4166 = CARTESIAN_POINT ( 'NONE',  ( 6.800000000000028244, -9.697272942313059056E-16, -3.000000000000000000 ) ) ;
#4167 = ORIENTED_EDGE ( 'NONE', *, *, #7818, .T. ) ;
#4168 =( NAMED_UNIT ( * ) SI_UNIT ( $, .STERADIAN. ) SOLID_ANGLE_UNIT ( ) );
#4169 = DIRECTION ( 'NONE',  ( -0.2425356250363328581, 0.9701425001453318764, 0.000000000000000000 ) ) ;
#4170 = ADVANCED_FACE ( 'NONE', ( #4434 ), #5514, .F. ) ;
#4171 = DIRECTION ( 'NONE',  ( 1.000000000000000000, 0.000000000000000000, 0.000000000000000000 ) ) ;
#4172 = AXIS2_PLACEMENT_3D ( 'NONE', #12610, #8221, #5945 ) ;
#4173 = ORIENTED_EDGE ( 'NONE', *, *, #3565, .T. ) ;
#4174 = CARTESIAN_POINT ( 'NONE',  ( 59.10586122665984732, -20.42344490663941414, -35.00000000000000000 ) ) ;
#4175 = ORIENTED_EDGE ( 'NONE', *, *, #9212, .F. ) ;
#4176 = VERTEX_POINT ( 'NONE', #159 ) ;
#4177 = DIRECTION ( 'NONE',  ( 0.000000000000000000, 0.000000000000000000, -1.000000000000000000 ) ) ;
#4178 = DIRECTION ( 'NONE',  ( -1.000000000000000000, 0.000000000000000000, 0.000000000000000000 ) ) ;
#4179 = AXIS2_PLACEMENT_3D ( 'NONE', #5845, #11291, #10184 ) ;
#4180 = CARTESIAN_POINT ( 'NONE',  ( 3.176101805495866071, 47.84421704054535240, 1.554735638783587337 ) ) ;
#4181 = EDGE_CURVE ( 'NONE', #1781, #3564, #10471, .T. ) ;
#4182 = DIRECTION ( 'NONE',  ( 0.000000000000000000, 0.000000000000000000, 1.000000000000000000 ) ) ;
#4183 = LINE ( 'NONE', #4260, #13140 ) ;
#4184 = SHAPE_DEFINITION_REPRESENTATION ( #2507, #11805 ) ;
#4185 = CARTESIAN_POINT ( 'NONE',  ( 4.630153689607063860, 0.000000000000000000, 0.000000000000000000 ) ) ;
#4186 = LINE ( 'NONE', #8628, #8199 ) ;
#4187 = PRODUCT_DEFINITION_SHAPE ( 'NONE', 'NONE',  #14488 ) ;
#4188 = ORIENTED_EDGE ( 'NONE', *, *, #6813, .F. ) ;
#4189 = ADVANCED_FACE ( 'NONE', ( #3536 ), #13565, .F. ) ;
#4190 = DIRECTION ( 'NONE',  ( -1.000000000000000000, 0.000000000000000000, 0.000000000000000000 ) ) ;
#4191 = ORIENTED_EDGE ( 'NONE', *, *, #5300, .T. ) ;
#4192 = AXIS2_PLACEMENT_3D ( 'NONE', #11228, #1207, #4589 ) ;
#4193 = ORIENTED_EDGE ( 'NONE', *, *, #13545, .T. ) ;
#4194 = AXIS2_PLACEMENT_3D ( 'NONE', #13226, #12189, #4101 ) ;
#4195 = ORIENTED_EDGE ( 'NONE', *, *, #13347, .T. ) ;
#4196 = CARTESIAN_POINT ( 'NONE',  ( 22.00000000000000000, 78.00000000000000000, 25.00000000000000000 ) ) ;
#4197 = CARTESIAN_POINT ( 'NONE',  ( 31.38313257588138683, 143.6985259526510674, 25.00000000000000000 ) ) ;
#4198 = EDGE_CURVE ( 'NONE', #661, #12838, #9522, .T. ) ;
#4199 = DIRECTION ( 'NONE',  ( 0.000000000000000000, 0.000000000000000000, -1.000000000000000000 ) ) ;
#4200 = EDGE_CURVE ( 'NONE', #13012, #8333, #12318, .T. ) ;
#4201 =( NAMED_UNIT ( * ) PLANE_ANGLE_UNIT ( ) SI_UNIT ( $, .RADIAN. ) );
#4202 =( GEOMETRIC_REPRESENTATION_CONTEXT ( 3 ) GLOBAL_UNCERTAINTY_ASSIGNED_CONTEXT ( ( #1331 ) ) GLOBAL_UNIT_ASSIGNED_CONTEXT ( ( #10231, #1025, #6793 ) ) REPRESENTATION_CONTEXT ( 'NONE', 'WORKASPACE' ) );
#4203 = EDGE_LOOP ( 'NONE', ( #1706, #10875, #1309, #3007 ) ) ;
#4204 = DIRECTION ( 'NONE',  ( -0.9701425001453318764, -0.2425356250363329969, 0.000000000000000000 ) ) ;
#4205 = CARTESIAN_POINT ( 'NONE',  ( -2.241758896820161572E-14, 5.987020429981935621, -4.630720594357044639 ) ) ;
#4206 = CARTESIAN_POINT ( 'NONE',  ( 0.000000000000000000, 0.000000000000000000, 0.000000000000000000 ) ) ;
#4207 = VECTOR ( 'NONE', #162, 1000.000000000000000 ) ;
#4208 = CARTESIAN_POINT ( 'NONE',  ( -8.000000000000000000, 25.49999999999996803, 0.000000000000000000 ) ) ;
#4209 = CYLINDRICAL_SURFACE ( 'NONE', #6670, 2.500000000000002220 ) ;
#4210 = LINE ( 'NONE', #2225, #2986 ) ;
#4211 = EDGE_CURVE ( 'NONE', #9931, #2739, #12738, .T. ) ;
#4212 = DIRECTION ( 'NONE',  ( -0.000000000000000000, 1.000000000000000000, 0.000000000000000000 ) ) ;
#4213 = CARTESIAN_POINT ( 'NONE',  ( 4.000000000000003553, 2.309401076758501592, -3.133295621305376422 ) ) ;
#4214 = AXIS2_PLACEMENT_3D ( 'NONE', #14132, #8251, #7076 ) ;
#4215 =( NAMED_UNIT ( * ) PLANE_ANGLE_UNIT ( ) SI_UNIT ( $, .RADIAN. ) );
#4216 = LINE ( 'NONE', #13000, #7509 ) ;
#4217 = VERTEX_POINT ( 'NONE', #8192 ) ;
#4218 = VERTEX_POINT ( 'NONE', #11413 ) ;
#4219 = CARTESIAN_POINT ( 'NONE',  ( 54.35294117647056567, -1.411764705882362358, -25.00000000000000000 ) ) ;
#4220 = EDGE_CURVE ( 'NONE', #10601, #12223, #11489, .T. ) ;
#4221 = CARTESIAN_POINT ( 'NONE',  ( 32.50229726637438432, 120.2985749985466839, 25.00000000000000000 ) ) ;
#4222 = CIRCLE ( 'NONE', #7930, 2.749999999999997780 ) ;
#4223 = ORIENTED_EDGE ( 'NONE', *, *, #4804, .F. ) ;
#4224 = DIRECTION ( 'NONE',  ( 1.000000000000000000, 0.000000000000000000, 0.000000000000000000 ) ) ;
#4225 = CARTESIAN_POINT ( 'NONE',  ( 68.68170757442801744, 29.57655509336062849, -106.9999999999999858 ) ) ;
#4226 = ORIENTED_EDGE ( 'NONE', *, *, #8091, .T. ) ;
#4227 = VECTOR ( 'NONE', #11402, 1000.000000000000000 ) ;
#4228 = ORIENTED_EDGE ( 'NONE', *, *, #11919, .F. ) ;
#4229 = ORIENTED_EDGE ( 'NONE', *, *, #9530, .T. ) ;
#4230 = CARTESIAN_POINT ( 'NONE',  ( 42.27836601746437850, 91.19429999418670718, -25.00000000000000000 ) ) ;
#4231 = DIRECTION ( 'NONE',  ( -1.000000000000000000, 0.000000000000000000, 0.000000000000000000 ) ) ;
#4232 = ORIENTED_EDGE ( 'NONE', *, *, #5600, .F. ) ;
#4233 = DIRECTION ( 'NONE',  ( 1.000000000000000000, 0.000000000000000000, 0.000000000000000000 ) ) ;
#4234 = FACE_OUTER_BOUND ( 'NONE', #3514, .T. ) ;
#4235 = EDGE_CURVE ( 'NONE', #13862, #6531, #12583, .T. ) ;
#4236 = EDGE_CURVE ( 'NONE', #1217, #777, #12455, .T. ) ;
#4237 = CYLINDRICAL_SURFACE ( 'NONE', #6021, 3.299999999999976730 ) ;
#4238 = CARTESIAN_POINT ( 'NONE',  ( 3.974183935050564997, -0.7239581970533717215, 3.565826011443126831 ) ) ;
#4239 = ORIENTED_EDGE ( 'NONE', *, *, #225, .F. ) ;
#4240 = FILL_AREA_STYLE ('',( #994 ) ) ;
#4241 = FACE_OUTER_BOUND ( 'NONE', #1147, .T. ) ;
#4242 = DIRECTION ( 'NONE',  ( 0.000000000000000000, 0.000000000000000000, -1.000000000000000000 ) ) ;
#4243 = VECTOR ( 'NONE', #11459, 1000.000000000000000 ) ;
#4244 = AXIS2_PLACEMENT_3D ( 'NONE', #7611, #2152, #20 ) ;
#4245 = ORIENTED_EDGE ( 'NONE', *, *, #13402, .T. ) ;
#4246 = EDGE_CURVE ( 'NONE', #8503, #3835, #6377, .T. ) ;
#4247 = ORIENTED_EDGE ( 'NONE', *, *, #75, .T. ) ;
#4248 = AXIS2_PLACEMENT_3D ( 'NONE', #3784, #12545, #10358 ) ;
#4249 = VERTEX_POINT ( 'NONE', #4908 ) ;
#4250 = DIRECTION ( 'NONE',  ( 0.000000000000000000, 0.000000000000000000, -1.000000000000000000 ) ) ;
#4251 = EDGE_LOOP ( 'NONE', ( #11878, #7206, #5369, #10185 ) ) ;
#4252 = CARTESIAN_POINT ( 'NONE',  ( 79.68170757442804586, 59.57655509336061073, -25.00000000000000000 ) ) ;
#4253 = ADVANCED_FACE ( 'NONE', ( #7976 ), #2428, .T. ) ;
#4254 = CARTESIAN_POINT ( 'NONE',  ( 5.248988766908546211, -2.532174945215656336, -4.566961984436638033 ) ) ;
#4255 = EDGE_CURVE ( 'NONE', #5614, #1477, #4700, .T. ) ;
#4256 = CARTESIAN_POINT ( 'NONE',  ( 118.6817075744280316, 109.5765550933604828, -3.299999999999983391 ) ) ;
#4257 = AXIS2_PLACEMENT_3D ( 'NONE', #2772, #13964, #12709 ) ;
#4258 = CARTESIAN_POINT ( 'NONE',  ( 39.70372226782770753, 81.49287499273339108, 25.00000000000000000 ) ) ;
#4259 = CIRCLE ( 'NONE', #12892, 3.000000000000000888 ) ;
#4260 = CARTESIAN_POINT ( 'NONE',  ( 20.00000000000000000, 80.00000000000000000, 25.00000000000000000 ) ) ;
#4261 = PRODUCT_CONTEXT ( 'NONE', #11289, 'mechanical' ) ;
#4262 = LINE ( 'NONE', #4569, #10065 ) ;
#4263 = VECTOR ( 'NONE', #4633, 1000.000000000000000 ) ;
#4264 = CARTESIAN_POINT ( 'NONE',  ( 4.158806965674310518, -4.075748668183996060, -0.05940377217585728065 ) ) ;
#4265 = EDGE_LOOP ( 'NONE', ( #2188, #13222, #7506, #10107 ) ) ;
#4266 = CARTESIAN_POINT ( 'NONE',  ( 4.158413352280787123, -2.044871626972824430, 3.541821552872963075 ) ) ;
#4267 = ADVANCED_FACE ( 'NONE', ( #6883 ), #10177, .T. ) ;
#4268 = VECTOR ( 'NONE', #2414, 1000.000000000000000 ) ;
#4269 = STYLED_ITEM ( 'NONE', ( #3540 ), #11166 ) ;
#4270 = VECTOR ( 'NONE', #8995, 999.9999999999998863 ) ;
#4271 = VERTEX_POINT ( 'NONE', #452 ) ;
#4272 = ORIENTED_EDGE ( 'NONE', *, *, #4676, .F. ) ;
#4273 = CARTESIAN_POINT ( 'NONE',  ( 3.667453972563985829E-15, 6.066067634115573703, -4.659491423763650886 ) ) ;
#4274 = CARTESIAN_POINT ( 'NONE',  ( 0.000000000000000000, -1.732050807568885631, 0.000000000000000000 ) ) ;
#4275 = CYLINDRICAL_SURFACE ( 'NONE', #2587, 2.749999999999997780 ) ;
#4276 = B_SPLINE_CURVE_WITH_KNOTS ( 'NONE', 3,
 ( #3833, #11797, #13926, #4055 ),
 .UNSPECIFIED., .F., .F.,
 ( 4, 4 ),
 ( 0.000000000000000000, 0.002080789711329273685 ),
 .UNSPECIFIED. ) ;
#4277 = DIRECTION ( 'NONE',  ( -1.000000000000000000, 0.000000000000000000, -0.000000000000000000 ) ) ;
#4278 = SURFACE_SIDE_STYLE ('',( #7672 ) ) ;
#4279 = AXIS2_PLACEMENT_3D ( 'NONE', #570, #8153, #491 ) ;
#4280 = EDGE_LOOP ( 'NONE', ( #5320, #13667 ) ) ;
#4281 = AXIS2_PLACEMENT_3D ( 'NONE', #8993, #1031, #10098 ) ;
#4282 = AXIS2_PLACEMENT_3D ( 'NONE', #5860, #10347, #4790 ) ;
#4283 = DIRECTION ( 'NONE',  ( 0.000000000000000000, -1.000000000000000000, 0.000000000000000000 ) ) ;
#4284 = LINE ( 'NONE', #2142, #8474 ) ;
#4285 = ADVANCED_FACE ( 'NONE', ( #9370 ), #13853, .T. ) ;
#4286 = CARTESIAN_POINT ( 'NONE',  ( 30.15499999999998693, 7.549649045036407798E-16, -2.499999999999999556 ) ) ;
#4287 = CARTESIAN_POINT ( 'NONE',  ( -4.140405595019058360, -2.228337868678527123, -3.386887224136953201 ) ) ;
#4288 = PRODUCT_DEFINITION_CONTEXT ( 'detailed design', #5115, 'design' ) ;
#4289 = CARTESIAN_POINT ( 'NONE',  ( -5.000000000000000000, 2.886751345948124214, -4.284345921091780696 ) ) ;
#4290 = CARTESIAN_POINT ( 'NONE',  ( 37.42765351673772045, 110.5971499970933536, -25.00000000000000000 ) ) ;
#4291 = DIRECTION ( 'NONE',  ( -1.000000000000000000, 2.551526159633733968E-19, 1.987661601597216239E-18 ) ) ;
#4292 = CARTESIAN_POINT ( 'NONE',  ( 20.00000000000000000, 60.00000000000000711, -25.00000000000000000 ) ) ;
#4293 = DIRECTION ( 'NONE',  ( 0.000000000000000000, 1.000000000000000000, 0.000000000000000000 ) ) ;
#4294 = DIRECTION ( 'NONE',  ( -1.000000000000000000, 0.000000000000000000, 0.000000000000000000 ) ) ;
#4295 = ORIENTED_EDGE ( 'NONE', *, *, #3565, .F. ) ;
#4296 = ORIENTED_EDGE ( 'NONE', *, *, #8889, .F. ) ;
#4297 = DIRECTION ( 'NONE',  ( 0.000000000000000000, 1.000000000000000000, 0.000000000000000000 ) ) ;
#4298 = AXIS2_PLACEMENT_3D ( 'NONE', #6530, #13153, #10725 ) ;
#4299 = CARTESIAN_POINT ( 'NONE',  ( 108.6817075744280743, 59.57655509336061073, -25.00000000000000000 ) ) ;
#4300 = VERTEX_POINT ( 'NONE', #7387 ) ;
#4301 = CARTESIAN_POINT ( 'NONE',  ( 3.370256023960729782E-15, 5.773502691896274186, -4.284345921091780696 ) ) ;
#4302 = ADVANCED_FACE ( 'NONE', ( #530, #10623, #11866 ), #8414, .T. ) ;
#4303 = CARTESIAN_POINT ( 'NONE',  ( 5.122341571230614399, -2.957385285031222111, -4.581776566113600957 ) ) ;
#4304 = EDGE_CURVE ( 'NONE', #1320, #6031, #1697, .T. ) ;
#4305 = VERTEX_POINT ( 'NONE', #10837 ) ;
#4306 = ORIENTED_EDGE ( 'NONE', *, *, #390, .T. ) ;
#4307 = PLANE ( 'NONE',  #9910 ) ;
#4308 = CARTESIAN_POINT ( 'NONE',  ( -0.5291067203508891259, 48.48680572720347470, 0.02618951120639553473 ) ) ;
#4309 = APPLICATION_CONTEXT ( 'automotive_design' ) ;
#4310 = ORIENTED_EDGE ( 'NONE', *, *, #6759, .F. ) ;
#4311 = DIRECTION ( 'NONE',  ( 0.000000000000000000, 1.000000000000000000, 0.000000000000000000 ) ) ;
#4312 = PLANE ( 'NONE',  #6074 ) ;
#4313 = PRODUCT_DEFINITION_SHAPE ( 'NONE', 'NONE',  #14491 ) ;
#4314 = DIRECTION ( 'NONE',  ( 0.000000000000000000, 0.000000000000000000, -1.000000000000000000 ) ) ;
#4315 = CARTESIAN_POINT ( 'NONE',  ( 3.880214671983573727, -0.7309020039786382483, 3.499999999999992895 ) ) ;
#4316 = EDGE_LOOP ( 'NONE', ( #12514, #13905, #3614, #4526, #7504, #7579, #8296, #13590, #5021, #4981, #11794, #2569 ) ) ;
#4317 =( LENGTH_UNIT ( ) NAMED_UNIT ( * ) SI_UNIT ( .MILLI., .METRE. ) );
#4318 = CARTESIAN_POINT ( 'NONE',  ( 0.000000000000000000, 0.000000000000000000, 0.000000000000000000 ) ) ;
#4319 = CARTESIAN_POINT ( 'NONE',  ( 88.22284556172391490, -83.66032599071898801, 28.00000000000000000 ) ) ;
#4320 =( GEOMETRIC_REPRESENTATION_CONTEXT ( 3 ) GLOBAL_UNCERTAINTY_ASSIGNED_CONTEXT ( ( #1317 ) ) GLOBAL_UNIT_ASSIGNED_CONTEXT ( ( #6135, #11556, #7081 ) ) REPRESENTATION_CONTEXT ( 'NONE', 'WORKASPACE' ) );
#4321 = ORIENTED_EDGE ( 'NONE', *, *, #6443, .F. ) ;
#4322 = ORIENTED_EDGE ( 'NONE', *, *, #4979, .F. ) ;
#4323 = AXIS2_PLACEMENT_3D ( 'NONE', #10259, #10188, #10055 ) ;
#4324 = FACE_OUTER_BOUND ( 'NONE', #3038, .T. ) ;
#4325 = EDGE_LOOP ( 'NONE', ( #4407, #1104, #13454 ) ) ;
#4326 = LINE ( 'NONE', #7645, #7461 ) ;
#4327 = CARTESIAN_POINT ( 'NONE',  ( 62.10586122665984732, -20.42344490663941414, 23.00000000000000000 ) ) ;
#4328 = CARTESIAN_POINT ( 'NONE',  ( 20.00000000000000000, 27.00000000000000355, -25.00000000000000000 ) ) ;
#4329 = DIRECTION ( 'NONE',  ( 0.000000000000000000, 0.000000000000000000, -1.000000000000000000 ) ) ;
#4330 = CARTESIAN_POINT ( 'NONE',  ( -2.750000000000003553, 40.49999999999999289, 8.000000000000007105 ) ) ;
#4331 = APPLICATION_PROTOCOL_DEFINITION ( 'draft international standard', 'automotive_design', 1998, #5305 ) ;
#4332 = DIRECTION ( 'NONE',  ( -0.7071067811865513475, 2.410276454430290041E-17, -0.7071067811865435759 ) ) ;
#4333 = ADVANCED_FACE ( 'NONE', ( #1613 ), #13925, .F. ) ;
#4334 = CARTESIAN_POINT ( 'NONE',  ( 4.158413352280787123, 2.044871626972824430, -3.541821552872970180 ) ) ;
#4335 = EDGE_LOOP ( 'NONE', ( #6126, #1610, #13908, #11375 ) ) ;
#4336 = DIRECTION ( 'NONE',  ( 0.000000000000000000, 0.8660254037844380415, 0.5000000000000011102 ) ) ;
#4337 = EDGE_CURVE ( 'NONE', #3729, #5373, #11505, .T. ) ;
#4338 = ORIENTED_EDGE ( 'NONE', *, *, #11968, .T. ) ;
#4339 = EDGE_CURVE ( 'NONE', #908, #55, #10340, .T. ) ;
#4340 = ORIENTED_EDGE ( 'NONE', *, *, #11879, .T. ) ;
#4341 = VERTEX_POINT ( 'NONE', #11796 ) ;
#4342 = CARTESIAN_POINT ( 'NONE',  ( -3.499999647538288627, 4.028415724610453275, -4.385927688751848130 ) ) ;
#4343 = DIRECTION ( 'NONE',  ( -1.000000000000000000, 0.000000000000000000, 0.000000000000000000 ) ) ;
#4344 = SHAPE_REPRESENTATION ( 'MirrorHardened Serrated Safety Wedge', ( #11025 ), #6837 ) ;
#4345 = CARTESIAN_POINT ( 'NONE',  ( 36.31750732272606541, 144.5765550933605823, 33.00000000000000000 ) ) ;
#4346 = CARTESIAN_POINT ( 'NONE',  ( 105.6817075744281311, 124.5765550933606107, -25.00000000000000000 ) ) ;
#4347 = FACE_BOUND ( 'NONE', #935, .T. ) ;
#4348 = EDGE_CURVE ( 'NONE', #630, #7481, #1944, .T. ) ;
#4349 = EDGE_LOOP ( 'NONE', ( #13755, #1986 ) ) ;
#4350 = DIRECTION ( 'NONE',  ( 0.000000000000000000, -1.000000000000000000, 0.000000000000000000 ) ) ;
#4351 = LINE ( 'NONE', #2489, #1223 ) ;
#4352 = EDGE_CURVE ( 'NONE', #13229, #9890, #8564, .T. ) ;
#4353 = FACE_OUTER_BOUND ( 'NONE', #9545, .T. ) ;
#4354 = CARTESIAN_POINT ( 'NONE',  ( -0.5449245075112842951, -4.304189842417356360, -3.016622336521895598 ) ) ;
#4355 = CARTESIAN_POINT ( 'NONE',  ( 4.686019787951672733, -3.464101615137762380, -1.999999999999994893 ) ) ;
#4356 = CARTESIAN_POINT ( 'NONE',  ( 5.108576461337678509, -4.721997478884301991, -0.02371338167649895967 ) ) ;
#4357 = CYLINDRICAL_SURFACE ( 'NONE', #2491, 2.500000000000002220 ) ;
#4358 = LINE ( 'NONE', #12877, #454 ) ;
#4359 = FACE_BOUND ( 'NONE', #1330, .T. ) ;
#4360 = VECTOR ( 'NONE', #8651, 1000.000000000000000 ) ;
#4361 = EDGE_CURVE ( 'NONE', #1377, #13885, #6147, .T. ) ;
#4362 = CARTESIAN_POINT ( 'NONE',  ( 58.68170757442803165, 29.57655509336062849, -28.00000000000000000 ) ) ;
#4363 = VERTEX_POINT ( 'NONE', #5125 ) ;
#4364 = CARTESIAN_POINT ( 'NONE',  ( -129.3408537872145132, 189.5765550933606107, -80.00000000000001421 ) ) ;
#4365 = FILL_AREA_STYLE ('',( #6825 ) ) ;
#4366 = EDGE_LOOP ( 'NONE', ( #2297, #9768, #13569, #7829 ) ) ;
#4367 = CARTESIAN_POINT ( 'NONE',  ( 5.103531824934171013, -4.708196996972898063, 1.387778780781445676E-14 ) ) ;
#4368 = EDGE_CURVE ( 'NONE', #5068, #2603, #812, .T. ) ;
#4369 = LINE ( 'NONE', #9013, #5204 ) ;
#4370 = EDGE_CURVE ( 'NONE', #768, #12696, #9669, .T. ) ;
#4371 = ORIENTED_EDGE ( 'NONE', *, *, #9778, .F. ) ;
#4372 = EDGE_LOOP ( 'NONE', ( #7484, #11615, #2605, #5588 ) ) ;
#4373 = VERTEX_POINT ( 'NONE', #7323 ) ;
#4374 = PLANE ( 'NONE',  #12974 ) ;
#4375 = CARTESIAN_POINT ( 'NONE',  ( -33.49999999999998579, 29.99999999999999645, 8.000000000000007105 ) ) ;
#4376 = CARTESIAN_POINT ( 'NONE',  ( 3.958484000407149761, -3.734437307742073386, -0.5317648453100152217 ) ) ;
#4377 = DIRECTION ( 'NONE',  ( 1.000000000000000000, 3.286707217423839940E-17, -2.273843122241290364E-18 ) ) ;
#4378 = FACE_OUTER_BOUND ( 'NONE', #6790, .T. ) ;
#4379 = ADVANCED_FACE ( 'NONE', ( #6221 ), #8335, .F. ) ;
#4380 = CARTESIAN_POINT ( 'NONE',  ( 4.055498735588713544, -1.410041617599688601, 3.568038744583310162 ) ) ;
#4381 = ORIENTED_EDGE ( 'NONE', *, *, #12499, .T. ) ;
#4382 = PRODUCT_RELATED_PRODUCT_CATEGORY ( 'part', '', ( #12552 ) ) ;
#4383 = EDGE_CURVE ( 'NONE', #2684, #619, #4527, .T. ) ;
#4384 = DIRECTION ( 'NONE',  ( 0.8191520442889913545, -4.865168473767734750E-47, 0.5735764363510468256 ) ) ;
#4385 = DIRECTION ( 'NONE',  ( 1.000000000000000000, -2.551526159633733968E-19, -1.987661601597216239E-18 ) ) ;
#4386 = AXIS2_PLACEMENT_3D ( 'NONE', #1114, #13274, #7545 ) ;
#4387 = ORIENTED_EDGE ( 'NONE', *, *, #944, .T. ) ;
#4388 = APPLICATION_CONTEXT ( 'automotive_design' ) ;
#4389 = ORIENTED_EDGE ( 'NONE', *, *, #5881, .F. ) ;
#4390 = ORIENTED_EDGE ( 'NONE', *, *, #5350, .F. ) ;
#4391 = CARTESIAN_POINT ( 'NONE',  ( 62.10586122665987574, -20.42344490663940704, 28.00000000000000000 ) ) ;
#4392 = EDGE_LOOP ( 'NONE', ( #12847, #6527, #12737, #7097 ) ) ;
#4393 = AXIS2_PLACEMENT_3D ( 'NONE', #11071, #13432, #8724 ) ;
#4394 = DIRECTION ( 'NONE',  ( -0.2425356250363328581, 0.9701425001453318764, 0.000000000000000000 ) ) ;
#4395 = CARTESIAN_POINT ( 'NONE',  ( 22.00000000000000000, 70.00000000000000000, -25.00000000000000000 ) ) ;
#4396 = DIRECTION ( 'NONE',  ( -1.000000000000000000, 4.625929269271485914E-16, 0.000000000000000000 ) ) ;
#4397 = CARTESIAN_POINT ( 'NONE',  ( 6.726859516510170778, 3.469446951953614189E-15, -4.900000000000015454 ) ) ;
#4398 = DIRECTION ( 'NONE',  ( 0.000000000000000000, 0.000000000000000000, -1.000000000000000000 ) ) ;
#4399 = DIRECTION ( 'NONE',  ( 1.000000000000000000, 0.000000000000000000, 0.000000000000000000 ) ) ;
#4400 = CYLINDRICAL_SURFACE ( 'NONE', #1439, 2.500000000000002220 ) ;
#4401 = CIRCLE ( 'NONE', #1110, 4.000000000000000888 ) ;
#4402 = EDGE_LOOP ( 'NONE', ( #224, #2364, #6078, #8375 ) ) ;
#4403 = VERTEX_POINT ( 'NONE', #681 ) ;
#4404 = ADVANCED_FACE ( 'NONE', ( #3029 ), #13123, .F. ) ;
#4405 = CARTESIAN_POINT ( 'NONE',  ( 0.000000000000000000, 25.49999999999996803, 8.000000000000007105 ) ) ;
#4406 = ORIENTED_EDGE ( 'NONE', *, *, #5896, .F. ) ;
#4407 = ORIENTED_EDGE ( 'NONE', *, *, #1816, .T. ) ;
#4408 = ORIENTED_EDGE ( 'NONE', *, *, #2646, .T. ) ;
#4409 = AXIS2_PLACEMENT_3D ( 'NONE', #13879, #3855, #11897 ) ;
#4410 = ORIENTED_EDGE ( 'NONE', *, *, #10256, .T. ) ;
#4411 = AXIS2_PLACEMENT_3D ( 'NONE', #7583, #5401, #12211 ) ;
#4412 = CARTESIAN_POINT ( 'NONE',  ( 3.499999647538293956, -4.028415724610476367, -4.385927688751854348 ) ) ;
#4413 = DIRECTION ( 'NONE',  ( -0.000000000000000000, -1.000000000000000000, -0.000000000000000000 ) ) ;
#4414 = FILL_AREA_STYLE_COLOUR ( '', #8162 ) ;
#4415 = CARTESIAN_POINT ( 'NONE',  ( 0.000000000000000000, 0.000000000000000000, 0.000000000000000000 ) ) ;
#4416 = ORIENTED_EDGE ( 'NONE', *, *, #4053, .T. ) ;
#4417 = FACE_OUTER_BOUND ( 'NONE', #1745, .T. ) ;
#4418 = CARTESIAN_POINT ( 'NONE',  ( 129.3408537872138595, 189.5765550933606107, -75.00000000000001421 ) ) ;
#4419 = DIRECTION ( 'NONE',  ( 1.000000000000000000, 0.000000000000000000, 0.000000000000000000 ) ) ;
#4420 = EDGE_CURVE ( 'NONE', #2086, #6626, #7300, .T. ) ;
#4421 = AXIS2_PLACEMENT_3D ( 'NONE', #11579, #12599, #10488 ) ;
#4422 = LINE ( 'NONE', #8852, #3320 ) ;
#4423 = EDGE_LOOP ( 'NONE', ( #11808, #3715, #558, #1090, #12995, #12520 ) ) ;
#4424 = VERTEX_POINT ( 'NONE', #12815 ) ;
#4425 = VECTOR ( 'NONE', #3395, 1000.000000000000000 ) ;
#4426 = FACE_OUTER_BOUND ( 'NONE', #5090, .T. ) ;
#4427 = VECTOR ( 'NONE', #10265, 1000.000000000000000 ) ;
#4428 = CARTESIAN_POINT ( 'NONE',  ( 27.75000000000001066, 2.516649172247811061E-16, -2.055000000000000160 ) ) ;
#4429 = VECTOR ( 'NONE', #13663, 1000.000000000000000 ) ;
#4430 = CARTESIAN_POINT ( 'NONE',  ( 54.35294117647056567, -1.411764705882362358, -23.00000000000000000 ) ) ;
#4431 = DIRECTION ( 'NONE',  ( 1.000000000000000000, -2.551526159633717598E-19, 1.734723475976770887E-18 ) ) ;
#4432 = SHAPE_REPRESENTATION ( 'link rod', ( #11025 ), #1200 ) ;
#4433 = ADVANCED_FACE ( 'NONE', ( #2800 ), #7240, .F. ) ;
#4434 = FACE_OUTER_BOUND ( 'NONE', #4127, .T. ) ;
#4435 = CARTESIAN_POINT ( 'NONE',  ( 42.12907851819100813, 71.79144999128007498, 25.00000000000000000 ) ) ;
#4436 = TOROIDAL_SURFACE ( 'NONE', #10955, 5.384454397937117776, 0.5155456020628805813 ) ;
#4437 = LINE ( 'NONE', #8794, #3533 ) ;
#4438 = EDGE_CURVE ( 'NONE', #10176, #6205, #13330, .T. ) ;
#4439 = CARTESIAN_POINT ( 'NONE',  ( 4.862837926274030664, -1.624916111836509858, 4.000000000000003553 ) ) ;
#4440 = ORIENTED_EDGE ( 'NONE', *, *, #6384, .F. ) ;
#4441 = VERTEX_POINT ( 'NONE', #8845 ) ;
#4442 = CARTESIAN_POINT ( 'NONE',  ( 3.951447005078477126, -3.704664227300094925, -0.5833333333333349247 ) ) ;
#4443 = ORIENTED_EDGE ( 'NONE', *, *, #3460, .F. ) ;
#4444 = CARTESIAN_POINT ( 'NONE',  ( 2.500000000000002220, 7.224953340212723619E-16, -4.674599999999973221 ) ) ;
#4445 = DIRECTION ( 'NONE',  ( 0.000000000000000000, 0.000000000000000000, -1.000000000000000000 ) ) ;
#4446 = ORIENTED_EDGE ( 'NONE', *, *, #7029, .F. ) ;
#4447 = EDGE_CURVE ( 'NONE', #10332, #6697, #232, .T. ) ;
#4448 = EDGE_LOOP ( 'NONE', ( #9190, #11549, #7257, #10824 ) ) ;
#4449 = AXIS2_PLACEMENT_3D ( 'NONE', #5324, #13310, #8550 ) ;
#4450 = FACE_OUTER_BOUND ( 'NONE', #3950, .T. ) ;
#4451 = CARTESIAN_POINT ( 'NONE',  ( 3.951447005078475350, -3.704664227300094037, 0.5833333333333315940 ) ) ;
#4452 = CARTESIAN_POINT ( 'NONE',  ( 3.972066048304797370, 2.740530939476389261, -2.384802634787859255 ) ) ;
#4453 = DIRECTION ( 'NONE',  ( 1.000000000000000000, 0.000000000000000000, 0.000000000000000000 ) ) ;
#4454 = PLANE ( 'NONE',  #9059 ) ;
#4455 = CARTESIAN_POINT ( 'NONE',  ( 0.000000000000000000, 0.000000000000000000, -4.699999999999981526 ) ) ;
#4456 = EDGE_LOOP ( 'NONE', ( #11312, #11868, #10925, #11480 ) ) ;
#4457 = AXIS2_PLACEMENT_3D ( 'NONE', #9749, #14301, #14375 ) ;
#4458 = CARTESIAN_POINT ( 'NONE',  ( 21.68170757442808849, 141.2731697022877313, 28.00000000000000000 ) ) ;
#4459 = AXIS2_PLACEMENT_3D ( 'NONE', #1095, #4485, #8919 ) ;
#4460 = CARTESIAN_POINT ( 'NONE',  ( 4.180231891692613111, 2.049421325483194778, 3.591231015387271519 ) ) ;
#4461 = ORIENTED_EDGE ( 'NONE', *, *, #10732, .F. ) ;
#4462 = EDGE_CURVE ( 'NONE', #1545, #9930, #14282, .T. ) ;
#4463 = ORIENTED_EDGE ( 'NONE', *, *, #13859, .T. ) ;
#4464 = AXIS2_PLACEMENT_3D ( 'NONE', #13909, #3881, #8316 ) ;
#4465 = DIRECTION ( 'NONE',  ( 1.000000000000000000, 0.000000000000000000, 0.000000000000000000 ) ) ;
#4466 = VERTEX_POINT ( 'NONE', #9803 ) ;
#4467 = LINE ( 'NONE', #1222, #720 ) ;
#4468 = FACE_OUTER_BOUND ( 'NONE', #306, .T. ) ;
#4469 = CYLINDRICAL_SURFACE ( 'NONE', #10965, 2.500000000000002220 ) ;
#4470 = CARTESIAN_POINT ( 'NONE',  ( 20.00000000000000000, 60.00000000000000711, 25.00000000000000000 ) ) ;
#4471 = CARTESIAN_POINT ( 'NONE',  ( -8.000000000000000000, 25.49999999999996803, 8.000000000000007105 ) ) ;
#4472 = CONTEXT_DEPENDENT_SHAPE_REPRESENTATION ( #3735, #6141 ) ;
#4473 = FACE_OUTER_BOUND ( 'NONE', #8579, .T. ) ;
#4474 = DIRECTION ( 'NONE',  ( 1.000000000000000000, 0.000000000000000000, 0.000000000000000000 ) ) ;
#4475 = AXIS2_PLACEMENT_3D ( 'NONE', #5801, #2539, #12775 ) ;
#4476 = DIRECTION ( 'NONE',  ( 0.000000000000000000, -1.000000000000000000, 0.000000000000000000 ) ) ;
#4477 = ORIENTED_EDGE ( 'NONE', *, *, #11688, .T. ) ;
#4478 = ADVANCED_FACE ( 'NONE', ( #1026 ), #2642, .T. ) ;
#4479 = DIRECTION ( 'NONE',  ( -0.2425356250363327748, 0.9701425001453319874, 0.000000000000000000 ) ) ;
#4480 = CIRCLE ( 'NONE', #11947, 2.500000000000009326 ) ;
#4481 = VERTEX_POINT ( 'NONE', #2052 ) ;
#4482 = CARTESIAN_POINT ( 'NONE',  ( 19.99999999999999645, 67.00000000000000000, -25.00000000000000000 ) ) ;
#4483 = VECTOR ( 'NONE', #1342, 1000.000000000000000 ) ;
#4484 = CARTESIAN_POINT ( 'NONE',  ( -5.000000000000001776, 1.953108124182664440, -0.2699991669428312147 ) ) ;
#4485 = DIRECTION ( 'NONE',  ( 0.000000000000000000, 0.000000000000000000, -1.000000000000000000 ) ) ;
#4486 = VECTOR ( 'NONE', #12915, 1000.000000000000000 ) ;
#4487 = DIRECTION ( 'NONE',  ( 0.000000000000000000, 0.000000000000000000, 1.000000000000000000 ) ) ;
#4488 = ADVANCED_FACE ( 'NONE', ( #2272 ), #943, .F. ) ;
#4489 = CARTESIAN_POINT ( 'NONE',  ( 4.939003118778963142, 2.662716476701372681, -3.388039776202472098 ) ) ;
#4490 = LINE ( 'NONE', #2344, #524 ) ;
#4491 = DIRECTION ( 'NONE',  ( -1.000000000000000000, -5.046468293750711996E-16, -1.680811587828860421E-31 ) ) ;
#4492 = DIRECTION ( 'NONE',  ( -1.000000000000000000, 0.000000000000000000, 0.000000000000000000 ) ) ;
#4493 = ORIENTED_EDGE ( 'NONE', *, *, #8944, .F. ) ;
#4494 = DIRECTION ( 'NONE',  ( 0.000000000000000000, 0.000000000000000000, -1.000000000000000000 ) ) ;
#4495 = AXIS2_PLACEMENT_3D ( 'NONE', #9513, #2792, #5112 ) ;
#4496 =( GEOMETRIC_REPRESENTATION_CONTEXT ( 3 ) GLOBAL_UNCERTAINTY_ASSIGNED_CONTEXT ( ( #3554 ) ) GLOBAL_UNIT_ASSIGNED_CONTEXT ( ( #6295, #13197, #5205 ) ) REPRESENTATION_CONTEXT ( 'NONE', 'WORKASPACE' ) );
#4497 = AXIS2_PLACEMENT_3D ( 'NONE', #4121, #8558, #13039 ) ;
#4498 = CARTESIAN_POINT ( 'NONE',  ( -3.081487911019577365E-30, 3.469446951953614189E-15, -6.000000000000005329 ) ) ;
#4499 =( REPRESENTATION_RELATIONSHIP ('NONE','NONE', #10295, #10940 ) REPRESENTATION_RELATIONSHIP_WITH_TRANSFORMATION ( #13315 )SHAPE_REPRESENTATION_RELATIONSHIP( ) );
#4500 = DIRECTION ( 'NONE',  ( 0.000000000000000000, 1.000000000000000000, 0.000000000000000000 ) ) ;
#4501 = EDGE_CURVE ( 'NONE', #5852, #6805, #11041, .T. ) ;
#4502 = CARTESIAN_POINT ( 'NONE',  ( 0.1410420225375863257, -4.700232803196146669, -3.387027626239156319 ) ) ;
#4503 = DIRECTION ( 'NONE',  ( -1.000000000000000000, 0.000000000000000000, 0.000000000000000000 ) ) ;
#4504 = CARTESIAN_POINT ( 'NONE',  ( -68.68170757442807428, 29.57655509336051125, -117.0000000000000000 ) ) ;
#4505 = FACE_OUTER_BOUND ( 'NONE', #12633, .T. ) ;
#4506 = AXIS2_PLACEMENT_3D ( 'NONE', #12154, #6580, #3523 ) ;
#4507 = AXIS2_PLACEMENT_3D ( 'NONE', #8324, #3963, #7151 ) ;
#4508 = CARTESIAN_POINT ( 'NONE',  ( 28.00000000000000355, 24.50000000000001421, 0.000000000000000000 ) ) ;
#4509 = EDGE_LOOP ( 'NONE', ( #6830, #2649, #794, #11026 ) ) ;
#4510 = DIRECTION ( 'NONE',  ( -2.273843122241288438E-18, -5.551115123125783935E-17, -1.000000000000000000 ) ) ;
#4511 = EDGE_LOOP ( 'NONE', ( #14276, #1496, #13998, #11944 ) ) ;
#4512 = PRESENTATION_LAYER_ASSIGNMENT (  '', '', ( #5426 ) ) ;
#4513 = LINE ( 'NONE', #1327, #1000 ) ;
#4514 = AXIS2_PLACEMENT_3D ( 'NONE', #7450, #9445, #807 ) ;
#4515 = EDGE_CURVE ( 'NONE', #6994, #7481, #4739, .T. ) ;
#4516 = EDGE_CURVE ( 'NONE', #10243, #10813, #13703, .T. ) ;
#4517 = EDGE_LOOP ( 'NONE', ( #1710, #3446, #11317, #853 ) ) ;
#4518 = VERTEX_POINT ( 'NONE', #1094 ) ;
#4519 = CARTESIAN_POINT ( 'NONE',  ( 47.12907851819101523, 71.79144999128007498, -25.00000000000000000 ) ) ;
#4520 = CARTESIAN_POINT ( 'NONE',  ( 19.99999999999999645, 57.00000000000000000, 25.00000000000000000 ) ) ;
#4521 = DIRECTION ( 'NONE',  ( 0.000000000000000000, -0.000000000000000000, 1.000000000000000000 ) ) ;
#4522 = DIRECTION ( 'NONE',  ( 0.000000000000000000, 0.000000000000000000, 1.000000000000000000 ) ) ;
#4523 = FACE_OUTER_BOUND ( 'NONE', #10701, .T. ) ;
#4524 = CARTESIAN_POINT ( 'NONE',  ( -0.6806757772000455731, 5.380514348698967275, -4.138711833383633909 ) ) ;
#4525 = AXIS2_PLACEMENT_3D ( 'NONE', #8204, #7028, #13716 ) ;
#4526 = ORIENTED_EDGE ( 'NONE', *, *, #9947, .F. ) ;
#4527 = CIRCLE ( 'NONE', #9159, 3.299999999999997158 ) ;
#4528 = DIRECTION ( 'NONE',  ( 0.000000000000000000, 0.000000000000000000, 1.000000000000000000 ) ) ;
#4529 = EDGE_LOOP ( 'NONE', ( #13408, #7556, #6699, #3004 ) ) ;
#4530 = CARTESIAN_POINT ( 'NONE',  ( 108.6817075744280743, 124.5765550933606107, -25.00000000000000000 ) ) ;
#4531 = EDGE_CURVE ( 'NONE', #10817, #4305, #873, .T. ) ;
#4532 = CARTESIAN_POINT ( 'NONE',  ( 60.00000000000000000, -6.123233995736768255E-16, 23.00000000000000000 ) ) ;
#4533 = ORIENTED_EDGE ( 'NONE', *, *, #10521, .T. ) ;
#4534 = ORIENTED_EDGE ( 'NONE', *, *, #4220, .T. ) ;
#4535 = AXIS2_PLACEMENT_3D ( 'NONE', #12310, #10981, #956 ) ;
#4536 = ORIENTED_EDGE ( 'NONE', *, *, #9120, .F. ) ;
#4537 = DIRECTION ( 'NONE',  ( -0.9240638205168503205, 0.3822382184081049017, 0.000000000000000000 ) ) ;
#4538 = ORIENTED_EDGE ( 'NONE', *, *, #10626, .T. ) ;
#4539 = DIRECTION ( 'NONE',  ( 0.000000000000000000, -1.000000000000000000, 0.000000000000000000 ) ) ;
#4540 = VECTOR ( 'NONE', #9648, 1000.000000000000000 ) ;
#4541 = CARTESIAN_POINT ( 'NONE',  ( -5.000000000000000000, -0.9835753746177068324, -0.05800540215398777844 ) ) ;
#4542 = CARTESIAN_POINT ( 'NONE',  ( 30.60000000000001563, 0.000000000000000000, 0.000000000000000000 ) ) ;
#4543 = DIRECTION ( 'NONE',  ( 1.000000000000000000, 0.000000000000000000, 0.000000000000000000 ) ) ;
#4544 = DIRECTION ( 'NONE',  ( 0.000000000000000000, -8.482162385747133845E-47, 1.000000000000000000 ) ) ;
#4545 = LINE ( 'NONE', #3437, #7980 ) ;
#4546 = CARTESIAN_POINT ( 'NONE',  ( 64.03192852109765454, -5.819950020346492892, 25.00000000000000000 ) ) ;
#4547 = EDGE_CURVE ( 'NONE', #6762, #5687, #4557, .T. ) ;
#4548 = CARTESIAN_POINT ( 'NONE',  ( 4.180345304246193550, -2.049116244671343789, 3.591763845239304143 ) ) ;
#4549 = CARTESIAN_POINT ( 'NONE',  ( 4.151274195509663478, -2.039912954708747339, 3.533232880573498047 ) ) ;
#4550 = AXIS2_PLACEMENT_3D ( 'NONE', #2919, #7356, #11831 ) ;
#4551 = ORIENTED_EDGE ( 'NONE', *, *, #58, .T. ) ;
#4552 = CARTESIAN_POINT ( 'NONE',  ( 57.35294117647057277, -1.411764705882362358, 25.00000000000000000 ) ) ;
#4553 = AXIS2_PLACEMENT_3D ( 'NONE', #1032, #13553, #5490 ) ;
#4554 = EDGE_LOOP ( 'NONE', ( #11599, #8685, #6383, #1863, #11350, #2894, #13470, #4387, #4158 ) ) ;
#4555 = ORIENTED_EDGE ( 'NONE', *, *, #4763, .F. ) ;
#4556 = DIRECTION ( 'NONE',  ( -1.000000000000000000, -1.913084959030911013E-15, -0.000000000000000000 ) ) ;
#4557 = LINE ( 'NONE', #10019, #10820 ) ;
#4558 = DIRECTION ( 'NONE',  ( -0.2425356250363328581, 0.9701425001453318764, 0.000000000000000000 ) ) ;
#4559 = FACE_OUTER_BOUND ( 'NONE', #970, .T. ) ;
#4560 = ORIENTED_EDGE ( 'NONE', *, *, #9668, .F. ) ;
#4561 = ADVANCED_BREP_SHAPE_REPRESENTATION ( '', ( #11635, #11025 ), #758 ) ;
#4562 = CARTESIAN_POINT ( 'NONE',  ( 76.68170757442801744, 29.57655509336063204, -33.00000000000000000 ) ) ;
#4564 = CIRCLE ( 'NONE', #4550, 2.499999999999999112 ) ;
#4563 = CARTESIAN_POINT ( 'NONE',  ( 0.000000000000000000, 0.000000000000000000, 0.000000000000000000 ) ) ;
#4565 = EDGE_CURVE ( 'NONE', #7705, #5395, #8918, .T. ) ;
#4566 = DIRECTION ( 'NONE',  ( -1.000000000000000000, 0.000000000000000000, 0.000000000000000000 ) ) ;
#4567 = ORIENTED_EDGE ( 'NONE', *, *, #6072, .T. ) ;
#4568 = EDGE_CURVE ( 'NONE', #1702, #12288, #12015, .T. ) ;
#4569 = CARTESIAN_POINT ( 'NONE',  ( 20.00000000000000000, 78.00000000000000000, -25.00000000000000000 ) ) ;
#4570 = CARTESIAN_POINT ( 'NONE',  ( -0.6666666666666672958, 4.233901974057265427, -3.000726591567076440 ) ) ;
#4571 = DIRECTION ( 'NONE',  ( 0.000000000000000000, 0.000000000000000000, 1.000000000000000000 ) ) ;
#4572 = VERTEX_POINT ( 'NONE', #7821 ) ;
#4573 = PRODUCT_DEFINITION_CONTEXT ( 'detailed design', #5305, 'design' ) ;
#4574 = CARTESIAN_POINT ( 'NONE',  ( 59.25585977000769589, 23.28432498401347672, 25.00000000000000000 ) ) ;
#4575 = DIRECTION ( 'NONE',  ( 0.000000000000000000, 0.000000000000000000, -1.000000000000000000 ) ) ;
#4576 = DIRECTION ( 'NONE',  ( -0.7071067811865513475, 0.000000000000000000, 0.7071067811865436870 ) ) ;
#4577 = CARTESIAN_POINT ( 'NONE',  ( 5.085140069777600580, 2.386564130380674165, 4.000000000000002665 ) ) ;
#4578 = VERTEX_POINT ( 'NONE', #12298 ) ;
#4579 = APPLICATION_CONTEXT ( 'automotive_design' ) ;
#4580 = DIRECTION ( 'NONE',  ( 0.000000000000000000, 0.000000000000000000, 1.000000000000000000 ) ) ;
#4581 = EDGE_LOOP ( 'NONE', ( #6415, #6070, #3516, #4003, #5735 ) ) ;
#4582 = CARTESIAN_POINT ( 'NONE',  ( 108.6817075744280743, -20.42344490663954204, -106.9999999999999858 ) ) ;
#4583 = ORIENTED_EDGE ( 'NONE', *, *, #2559, .T. ) ;
#4584 = DIRECTION ( 'NONE',  ( 1.000000000000000000, 0.000000000000000000, -0.000000000000000000 ) ) ;
#4585 = CARTESIAN_POINT ( 'NONE',  ( 59.18121602037099649, 13.58289998256015352, 25.00000000000000000 ) ) ;
#4586 = FACE_OUTER_BOUND ( 'NONE', #265, .T. ) ;
#4587 = LINE ( 'NONE', #13510, #8999 ) ;
#4588 = CARTESIAN_POINT ( 'NONE',  ( 31.80000000000005045, 6.063261456088593708E-15, -2.445499999999972474 ) ) ;
#4589 = DIRECTION ( 'NONE',  ( -1.000000000000000000, 0.000000000000000000, 0.000000000000000000 ) ) ;
#4590 = DIRECTION ( 'NONE',  ( -1.000000000000000000, -3.286707217423839940E-17, -2.273843122241288053E-18 ) ) ;
#4591 = EDGE_CURVE ( 'NONE', #11701, #8874, #11748, .T. ) ;
#4592 = ORIENTED_EDGE ( 'NONE', *, *, #7191, .F. ) ;
#4593 = LINE ( 'NONE', #8002, #8820 ) ;
#4594 = DIRECTION ( 'NONE',  ( 0.000000000000000000, 0.000000000000000000, 1.000000000000000000 ) ) ;
#4595 = ORIENTED_EDGE ( 'NONE', *, *, #7703, .F. ) ;
#4596 = EDGE_CURVE ( 'NONE', #10542, #3192, #12932, .T. ) ;
#4597 = ORIENTED_EDGE ( 'NONE', *, *, #1244, .T. ) ;
#4598 = ORIENTED_EDGE ( 'NONE', *, *, #12458, .F. ) ;
#4599 = CARTESIAN_POINT ( 'NONE',  ( 0.000000000000000000, 0.000000000000000000, -4.674599999999973221 ) ) ;
#4600 = EDGE_CURVE ( 'NONE', #4518, #1328, #13764, .T. ) ;
#4601 = EDGE_LOOP ( 'NONE', ( #10210, #5875, #830, #7535 ) ) ;
#4602 = DIRECTION ( 'NONE',  ( 0.000000000000000000, 0.000000000000000000, 1.000000000000000000 ) ) ;
#4603 = CARTESIAN_POINT ( 'NONE',  ( 5.000000000000001776, 1.026510551521092385, -4.269855120319423492 ) ) ;
#4604 = LINE ( 'NONE', #7808, #915 ) ;
#4605 = DIRECTION ( 'NONE',  ( 1.000000000000000000, 1.665334536937734071E-16, 0.000000000000000000 ) ) ;
#4606 = CARTESIAN_POINT ( 'NONE',  ( 42.20372226782770753, 81.49287499273339108, 25.00000000000000000 ) ) ;
#4607 = CONTEXT_DEPENDENT_SHAPE_REPRESENTATION ( #2238, #99 ) ;
#4608 = EDGE_CURVE ( 'NONE', #13561, #6548, #14104, .T. ) ;
#4609 = CARTESIAN_POINT ( 'NONE',  ( -2.540000000000002700, -1.119346853987568578E-16, 1.599999999999990319 ) ) ;
#4610 = CARTESIAN_POINT ( 'NONE',  ( 4.086376042167603195, -1.979461949354205164, 3.571471332069175997 ) ) ;
#4611 = VECTOR ( 'NONE', #10707, 1000.000000000000000 ) ;
#4612 = ORIENTED_EDGE ( 'NONE', *, *, #10257, .T. ) ;
#4613 = DIRECTION ( 'NONE',  ( -0.2425356250363328581, 0.9701425001453318764, 0.000000000000000000 ) ) ;
#4614 = EDGE_CURVE ( 'NONE', #14288, #568, #5133, .T. ) ;
#4615 = CARTESIAN_POINT ( 'NONE',  ( 0.4318028594007592424, -5.811705888749004956, -4.566911319714220596 ) ) ;
#4616 = FACE_OUTER_BOUND ( 'NONE', #5685, .T. ) ;
#4617 = CARTESIAN_POINT ( 'NONE',  ( -5.236775389869354314, -1.020994252193095253, -4.356146547543389147 ) ) ;
#4618 = CARTESIAN_POINT ( 'NONE',  ( 58.68170757442803165, 39.57655509336063204, -33.00000000000000000 ) ) ;
#4619 = AXIS2_PLACEMENT_3D ( 'NONE', #8664, #13007, #4154 ) ;
#4620 = ORIENTED_EDGE ( 'NONE', *, *, #3213, .F. ) ;
#4621 = PLANE ( 'NONE',  #4281 ) ;
#4622 = AXIS2_PLACEMENT_3D ( 'NONE', #2398, #1225, #7873 ) ;
#4623 = DIRECTION ( 'NONE',  ( 0.000000000000000000, 0.000000000000000000, -1.000000000000000000 ) ) ;
#4624 = DIRECTION ( 'NONE',  ( 0.000000000000000000, 0.000000000000000000, -1.000000000000000000 ) ) ;
#4625 = ORIENTED_EDGE ( 'NONE', *, *, #8617, .T. ) ;
#4626 = PRODUCT_DEFINITION_SHAPE ( 'NONE', 'NONE',  #14465 ) ;
#4627 = PLANE ( 'NONE',  #13165 ) ;
#4628 = CIRCLE ( 'NONE', #1830, 2.100000000000000977 ) ;
#4629 = EDGE_LOOP ( 'NONE', ( #4869, #1192 ) ) ;
#4630 = EDGE_CURVE ( 'NONE', #4679, #1857, #1374, .T. ) ;
#4631 = EDGE_CURVE ( 'NONE', #3492, #1128, #13010, .T. ) ;
#4632 = CARTESIAN_POINT ( 'NONE',  ( -1.752700365193367750E-15, -5.773502691896304384, -4.284345921091780696 ) ) ;
#4633 = DIRECTION ( 'NONE',  ( 0.000000000000000000, 0.000000000000000000, -1.000000000000000000 ) ) ;
#4634 = AXIS2_PLACEMENT_3D ( 'NONE', #1322, #2578, #2433 ) ;
#4635 = VECTOR ( 'NONE', #4650, 1000.000000000000114 ) ;
#4636 = AXIS2_PLACEMENT_3D ( 'NONE', #7038, #13876, #10415 ) ;
#4637 = VERTEX_POINT ( 'NONE', #7003 ) ;
#4638 = VECTOR ( 'NONE', #5311, 1000.000000000000000 ) ;
#4639 = CARTESIAN_POINT ( 'NONE',  ( 4.175813232069169878, -2.061359961916378492, -3.570380186727409200 ) ) ;
#4640 = EDGE_LOOP ( 'NONE', ( #8368, #1419, #13334, #100, #2245, #754, #3343, #7325 ) ) ;
#4641 = FACE_OUTER_BOUND ( 'NONE', #12693, .T. ) ;
#4642 = AXIS2_PLACEMENT_3D ( 'NONE', #7297, #4242, #11772 ) ;
#4643 = EDGE_LOOP ( 'NONE', ( #12354, #6102, #5914, #12049 ) ) ;
#4644 = VECTOR ( 'NONE', #12554, 1000.000000000000000 ) ;
#4645 = EDGE_CURVE ( 'NONE', #4911, #7523, #9497, .T. ) ;
#4646 = DIRECTION ( 'NONE',  ( -1.000000000000000000, 0.000000000000000000, 0.000000000000000000 ) ) ;
#4647 = CARTESIAN_POINT ( 'NONE',  ( 4.071447262713911996, -2.020725942163681399, 3.499999999999989342 ) ) ;
#4648 = CIRCLE ( 'NONE', #3958, 6.726859516510133474 ) ;
#4649 = DIRECTION ( 'NONE',  ( 1.000000000000000000, -0.000000000000000000, -0.000000000000000000 ) ) ;
#4650 = DIRECTION ( 'NONE',  ( -0.2425356250363328581, 0.9701425001453318764, 0.000000000000000000 ) ) ;
#4651 = DIRECTION ( 'NONE',  ( 0.000000000000000000, 1.000000000000000000, 0.000000000000000000 ) ) ;
#4652 = DIRECTION ( 'NONE',  ( 0.000000000000000000, 0.000000000000000000, 1.000000000000000000 ) ) ;
#4653 = ORIENTED_EDGE ( 'NONE', *, *, #11313, .F. ) ;
#4654 = CARTESIAN_POINT ( 'NONE',  ( 0.000000000000000000, 0.000000000000000000, -0.3851141460153306717 ) ) ;
#4655 = ORIENTED_EDGE ( 'NONE', *, *, #3657, .F. ) ;
#4656 = DIRECTION ( 'NONE',  ( 0.000000000000000000, -1.000000000000000000, 0.000000000000000000 ) ) ;
#4657 = AXIS2_PLACEMENT_3D ( 'NONE', #11310, #10351, #12607 ) ;
#4658 = ORIENTED_EDGE ( 'NONE', *, *, #8473, .F. ) ;
#4659 = CARTESIAN_POINT ( 'NONE',  ( 5.108576461337681174, -2.340462348500684353, -4.101226464158124863 ) ) ;
#4660 = ORIENTED_EDGE ( 'NONE', *, *, #522, .F. ) ;
#4661 = EDGE_CURVE ( 'NONE', #6344, #11445, #7059, .T. ) ;
#4662 = ORIENTED_EDGE ( 'NONE', *, *, #11245, .T. ) ;
#4663 = EDGE_CURVE ( 'NONE', #4769, #55, #12642, .T. ) ;
#4664 = CARTESIAN_POINT ( 'NONE',  ( 5.099999999999993427, 0.000000000000000000, 0.000000000000000000 ) ) ;
#4665 = ORIENTED_EDGE ( 'NONE', *, *, #13305, .F. ) ;
#4666 = CARTESIAN_POINT ( 'NONE',  ( -3.081487911019577365E-30, 3.469446951953614189E-15, -5.432899837730820636 ) ) ;
#4667 = VECTOR ( 'NONE', #134, 1000.000000000000000 ) ;
#4668 = CARTESIAN_POINT ( 'NONE',  ( 5.000000000000001776, -2.119125225736587570, -4.142110484952109317 ) ) ;
#4669 = FILL_AREA_STYLE_COLOUR ( '', #10254 ) ;
#4670 = DIRECTION ( 'NONE',  ( 0.000000000000000000, 0.000000000000000000, 1.000000000000000000 ) ) ;
#4671 = DIRECTION ( 'NONE',  ( 0.000000000000000000, 0.000000000000000000, -1.000000000000000000 ) ) ;
#4672 = VECTOR ( 'NONE', #10448, 1000.000000000000000 ) ;
#4673 = DIRECTION ( 'NONE',  ( -1.000000000000000000, 0.000000000000000000, 0.000000000000000000 ) ) ;
#4674 = CARTESIAN_POINT ( 'NONE',  ( -4.211399291375520271, 2.459730787265050900, -3.451162385478133476 ) ) ;
#4675 = FACE_OUTER_BOUND ( 'NONE', #5880, .T. ) ;
#4676 = EDGE_CURVE ( 'NONE', #1176, #12547, #2633, .T. ) ;
#4677 = EDGE_CURVE ( 'NONE', #12519, #10509, #12570, .T. ) ;
#4678 = VECTOR ( 'NONE', #10003, 1000.000000000000000 ) ;
#4679 = VERTEX_POINT ( 'NONE', #214 ) ;
#4680 = VERTEX_POINT ( 'NONE', #2480 ) ;
#4681 = EDGE_CURVE ( 'NONE', #14168, #3573, #7075, .T. ) ;
#4682 = LINE ( 'NONE', #9200, #8961 ) ;
#4683 = ORIENTED_EDGE ( 'NONE', *, *, #12732, .T. ) ;
#4684 = EDGE_CURVE ( 'NONE', #2270, #4092, #10888, .T. ) ;
#4685 = VERTEX_POINT ( 'NONE', #10447 ) ;
#4686 = CARTESIAN_POINT ( 'NONE',  ( 20.00000000000000000, 80.00000000000000000, 25.00000000000000000 ) ) ;
#4687 = CARTESIAN_POINT ( 'NONE',  ( -5.000000000000000000, -1.044998857007659154, -4.017857204714943897 ) ) ;
#4688 = CARTESIAN_POINT ( 'NONE',  ( 5.551115123125782702E-14, -3.464101615137743728, 2.000000000000001776 ) ) ;
#4689 = FACE_OUTER_BOUND ( 'NONE', #4905, .T. ) ;
#4690 = FILL_AREA_STYLE ('',( #3454 ) ) ;
#4691 = DIRECTION ( 'NONE',  ( 0.000000000000000000, 1.000000000000000000, 0.000000000000000000 ) ) ;
#4692 = ORIENTED_EDGE ( 'NONE', *, *, #13091, .F. ) ;
#4693 = EDGE_CURVE ( 'NONE', #11306, #2267, #438, .T. ) ;
#4694 = LINE ( 'NONE', #9364, #13633 ) ;
#4695 = ORIENTED_EDGE ( 'NONE', *, *, #7835, .T. ) ;
#4696 = VECTOR ( 'NONE', #1747, 1000.000000000000000 ) ;
#4697 = MECHANICAL_DESIGN_GEOMETRIC_PRESENTATION_REPRESENTATION (  '', ( #6068 ), #5387 ) ;
#4698 = ORIENTED_EDGE ( 'NONE', *, *, #8453, .T. ) ;
#4699 = VECTOR ( 'NONE', #6233, 1000.000000000000000 ) ;
#4700 = LINE ( 'NONE', #7092, #5532 ) ;
#4701 = CARTESIAN_POINT ( 'NONE',  ( 19.99999999999999645, 67.00000000000000000, 25.00000000000000000 ) ) ;
#4702 = VECTOR ( 'NONE', #7007, 1000.000000000000000 ) ;
#4703 = ORIENTED_EDGE ( 'NONE', *, *, #5569, .T. ) ;
#4704 = STYLED_ITEM ( 'NONE', ( #5314 ), #11715 ) ;
#4705 = ORIENTED_EDGE ( 'NONE', *, *, #1873, .T. ) ;
#4706 = CARTESIAN_POINT ( 'NONE',  ( 0.000000000000000000, 0.000000000000000000, 0.000000000000000000 ) ) ;
#4707 = EDGE_CURVE ( 'NONE', #4842, #9976, #6795, .T. ) ;
#4708 = VECTOR ( 'NONE', #2496, 1000.000000000000000 ) ;
#4709 = LINE ( 'NONE', #1621, #3330 ) ;
#4710 = CARTESIAN_POINT ( 'NONE',  ( -5.000000000000001776, -2.886751345948152192, -4.284345921091780696 ) ) ;
#4711 = VERTEX_POINT ( 'NONE', #12439 ) ;
#4712 = AXIS2_PLACEMENT_3D ( 'NONE', #6706, #12283, #10154 ) ;
#4713 = UNCERTAINTY_MEASURE_WITH_UNIT (LENGTH_MEASURE( 1.000000000000000082E-05 ), #5031, 'distance_accuracy_value', 'NONE');
#4714 = AXIS2_PLACEMENT_3D ( 'NONE', #5268, #11858, #7313 ) ;
#4715 = PLANE ( 'NONE',  #3607 ) ;
#4716 = DIRECTION ( 'NONE',  ( -1.000000000000000000, 0.000000000000000000, 0.000000000000000000 ) ) ;
#4717 = PLANE ( 'NONE',  #3072 ) ;
#4718 = LINE ( 'NONE', #11740, #1834 ) ;
#4719 = SURFACE_SIDE_STYLE ('',( #12473 ) ) ;
#4720 = CARTESIAN_POINT ( 'NONE',  ( 22.00000000000000000, 60.00000000000000711, -25.00000000000000000 ) ) ;
#4721 = DIRECTION ( 'NONE',  ( 1.000000000000000000, 0.000000000000000000, 0.000000000000000000 ) ) ;
#4722 = VERTEX_POINT ( 'NONE', #1240 ) ;
#4723 =( NAMED_UNIT ( * ) SI_UNIT ( $, .STERADIAN. ) SOLID_ANGLE_UNIT ( ) );
#4724 = EDGE_LOOP ( 'NONE', ( #10248, #3408, #10323, #7341 ) ) ;
#4725 = DIRECTION ( 'NONE',  ( 0.000000000000000000, 0.000000000000000000, -1.000000000000000000 ) ) ;
#4726 = AXIS2_PLACEMENT_3D ( 'NONE', #6179, #10651, #8445 ) ;
#4727 = EDGE_CURVE ( 'NONE', #11896, #663, #149, .T. ) ;
#4728 = AXIS2_PLACEMENT_3D ( 'NONE', #14203, #1604, #8486 ) ;
#4729 = ADVANCED_FACE ( 'NONE', ( #4616 ), #9057, .T. ) ;
#4730 = CARTESIAN_POINT ( 'NONE',  ( 129.3408537872138595, 199.5765550933606107, -9.000000000000007105 ) ) ;
#4731 = VERTEX_POINT ( 'NONE', #7629 ) ;
#4732 = CARTESIAN_POINT ( 'NONE',  ( 31.41872415839353039, 143.5561596226025074, -28.00000000000000000 ) ) ;
#4733 = ORIENTED_EDGE ( 'NONE', *, *, #10431, .F. ) ;
#4734 = ORIENTED_EDGE ( 'NONE', *, *, #390, .F. ) ;
#4735 = DIRECTION ( 'NONE',  ( 0.000000000000000000, 8.482162385747133845E-47, -1.000000000000000000 ) ) ;
#4736 = LINE ( 'NONE', #12701, #10795 ) ;
#4737 = CARTESIAN_POINT ( 'NONE',  ( 33.99999999999998579, 80.00000000000000000, -25.00000000000000000 ) ) ;
#4738 = CIRCLE ( 'NONE', #13393, 9.999999999999996447 ) ;
#4739 = CIRCLE ( 'NONE', #302, 4.000000000000004441 ) ;
#4740 = PRODUCT_DEFINITION_SHAPE ( 'NONE', 'NONE',  #14477 ) ;
#4741 = CARTESIAN_POINT ( 'NONE',  ( 0.000000000000000000, -4.618802153517030717, -4.699999999999981526 ) ) ;
#4742 = CARTESIAN_POINT ( 'NONE',  ( 118.6817075744280316, 69.57655509336046862, -3.299999999999983391 ) ) ;
#4743 = DIRECTION ( 'NONE',  ( 0.000000000000000000, 0.000000000000000000, -1.000000000000000000 ) ) ;
#4744 = ORIENTED_EDGE ( 'NONE', *, *, #1617, .T. ) ;
#4745 = CARTESIAN_POINT ( 'NONE',  ( 0.3126073911696169993, 4.041451884327390331, 0.000000000000000000 ) ) ;
#4746 = DIRECTION ( 'NONE',  ( -1.000000000000000000, 0.000000000000000000, 0.000000000000000000 ) ) ;
#4747 = CARTESIAN_POINT ( 'NONE',  ( 37.42765351673772045, 110.5971499970933536, 25.00000000000000000 ) ) ;
#4748 = CARTESIAN_POINT ( 'NONE',  ( 5.000000000000001776, -0.4954705650270038175, -7.013432803265606807E-16 ) ) ;
#4749 = VECTOR ( 'NONE', #3261, 1000.000000000000000 ) ;
#4750 = ORIENTED_EDGE ( 'NONE', *, *, #12459, .F. ) ;
#4751 = CARTESIAN_POINT ( 'NONE',  ( 2.426025403784448642, 2.655529440325959183E-32, -2.168404344971008868E-16 ) ) ;
#4752 = ORIENTED_EDGE ( 'NONE', *, *, #1593, .T. ) ;
#4753 = DIRECTION ( 'NONE',  ( -0.000000000000000000, 1.000000000000000000, -0.000000000000000000 ) ) ;
#4754 = DIRECTION ( 'NONE',  ( 0.000000000000000000, 0.000000000000000000, -1.000000000000000000 ) ) ;
#4755 = CARTESIAN_POINT ( 'NONE',  ( 56.99999999999997868, -9.797174393178845379E-16, 25.00000000000000000 ) ) ;
#4756 = FACE_OUTER_BOUND ( 'NONE', #10146, .T. ) ;
#4757 = CIRCLE ( 'NONE', #8495, 2.055000000000000160 ) ;
#4758 = ORIENTED_EDGE ( 'NONE', *, *, #7735, .T. ) ;
#4759 = DIRECTION ( 'NONE',  ( -1.000000000000000000, 0.000000000000000000, 0.000000000000000000 ) ) ;
#4760 = DIRECTION ( 'NONE',  ( 0.000000000000000000, 0.000000000000000000, -1.000000000000000000 ) ) ;
#4761 = FACE_OUTER_BOUND ( 'NONE', #5259, .T. ) ;
#4762 = VECTOR ( 'NONE', #7302, 1000.000000000000000 ) ;
#4763 = EDGE_CURVE ( 'NONE', #6682, #8106, #1679, .T. ) ;
#4764 = ADVANCED_FACE ( 'NONE', ( #13225 ), #4312, .F. ) ;
#4765 = LINE ( 'NONE', #2720, #3110 ) ;
#4766 = ORIENTED_EDGE ( 'NONE', *, *, #10539, .T. ) ;
#4767 = ORIENTED_EDGE ( 'NONE', *, *, #4707, .T. ) ;
#4768 = ORIENTED_EDGE ( 'NONE', *, *, #7085, .T. ) ;
#4769 = VERTEX_POINT ( 'NONE', #12051 ) ;
#4770 = VECTOR ( 'NONE', #3863, 1000.000000000000000 ) ;
#4771 = DIRECTION ( 'NONE',  ( 0.000000000000000000, 0.000000000000000000, -1.000000000000000000 ) ) ;
#4772 = CARTESIAN_POINT ( 'NONE',  ( 0.000000000000000000, 40.49999999999999289, 8.000000000000007105 ) ) ;
#4773 = EDGE_CURVE ( 'NONE', #2554, #13711, #2135, .T. ) ;
#4774 = B_SPLINE_CURVE_WITH_KNOTS ( 'NONE', 3,
 ( #13786, #11571, #3548, #13713, #8122, #12744, #2657, #386, #3617, #5926, #9455, #5847, #8202, #6887, #316, #11647 ),
 .UNSPECIFIED., .F., .F.,
 ( 4, 3, 3, 3, 3, 4 ),
 ( -2.214559098553098548E-06, 0.000000000000000000, 3.881464059293194212E-05, 7.921402936568228050E-05, 0.0001155901529638607309, 0.0001522174276055590983 ),
 .UNSPECIFIED. ) ;
#4775 = ADVANCED_FACE ( 'NONE', ( #3199 ), #12723, .T. ) ;
#4776 = ORIENTED_EDGE ( 'NONE', *, *, #53, .T. ) ;
#4777 = CARTESIAN_POINT ( 'NONE',  ( 0.000000000000000000, 40.49999999999999289, 8.000000000000007105 ) ) ;
#4778 = CARTESIAN_POINT ( 'NONE',  ( 60.00000000000000000, -6.123233995736768255E-16, -25.00000000000000000 ) ) ;
#4779 = ORIENTED_EDGE ( 'NONE', *, *, #6806, .F. ) ;
#4780 = DIRECTION ( 'NONE',  ( 0.000000000000000000, -0.4999999999999997224, 0.8660254037844387076 ) ) ;
#4781 = ORIENTED_EDGE ( 'NONE', *, *, #8707, .T. ) ;
#4782 = CARTESIAN_POINT ( 'NONE',  ( -0.6507732100473486714, 4.243078065514781727, -0.2236248678334887274 ) ) ;
#4783 = LINE ( 'NONE', #13658, #7540 ) ;
#4784 = ORIENTED_EDGE ( 'NONE', *, *, #6220, .F. ) ;
#4785 = ADVANCED_FACE ( 'NONE', ( #9508 ), #10872, .F. ) ;
#4786 = CARTESIAN_POINT ( 'NONE',  ( -4.597743007729438780, -3.118994528718963988, -0.4198507760575687642 ) ) ;
#4787 = FACE_OUTER_BOUND ( 'NONE', #9061, .T. ) ;
#4788 = FILL_AREA_STYLE_COLOUR ( '', #285 ) ;
#4789 = CARTESIAN_POINT ( 'NONE',  ( -0.1702248550645321934, 5.871782057790553289, -4.589066185948677656 ) ) ;
#4790 = DIRECTION ( 'NONE',  ( 0.000000000000000000, 0.000000000000000000, -1.000000000000000000 ) ) ;
#4791 = ORIENTED_EDGE ( 'NONE', *, *, #6813, .T. ) ;
#4792 = DIRECTION ( 'NONE',  ( 0.000000000000000000, 0.000000000000000000, -1.000000000000000000 ) ) ;
#4793 = EDGE_CURVE ( 'NONE', #6532, #2424, #10708, .T. ) ;
#4794 = CARTESIAN_POINT ( 'NONE',  ( 1.287221018261892169, 3.875624752116891614, -3.130620751971864291 ) ) ;
#4795 = ORIENTED_EDGE ( 'NONE', *, *, #5526, .T. ) ;
#4796 = CARTESIAN_POINT ( 'NONE',  ( 4.211140560182194292, -2.431303136016548017, -3.445885042887453231 ) ) ;
#4797 = CARTESIAN_POINT ( 'NONE',  ( 4.942464816486673129, 2.653516201069836988, 3.403975121041074026 ) ) ;
#4798 = EDGE_LOOP ( 'NONE', ( #1802, #12381, #9453, #10952 ) ) ;
#4799 = CARTESIAN_POINT ( 'NONE',  ( 5.035982117295163540, 4.629472459842971510, 2.352375968396500403E-18 ) ) ;
#4800 = ORIENTED_EDGE ( 'NONE', *, *, #381, .F. ) ;
#4801 = ORIENTED_EDGE ( 'NONE', *, *, #2205, .T. ) ;
#4802 = LINE ( 'NONE', #12113, #9681 ) ;
#4803 = CARTESIAN_POINT ( 'NONE',  ( 0.000000000000000000, 48.49999999999999289, 8.000000000000007105 ) ) ;
#4804 = EDGE_CURVE ( 'NONE', #8584, #9446, #6536, .T. ) ;
#4805 = CARTESIAN_POINT ( 'NONE',  ( 0.3572655899081733644, -2.309401076758484272, 4.000000000000031086 ) ) ;
#4806 = EDGE_CURVE ( 'NONE', #6304, #5931, #13085, .T. ) ;
#4807 = CARTESIAN_POINT ( 'NONE',  ( 4.872112557122744825, 2.415041619695410755E-11, 4.072377784234180176 ) ) ;
#4808 = CARTESIAN_POINT ( 'NONE',  ( -108.6817075744279748, -20.42344490663957046, 33.00000000000002842 ) ) ;
#4809 = CARTESIAN_POINT ( 'NONE',  ( 0.000000000000000000, 0.000000000000000000, 2.400000000000013234 ) ) ;
#4810 = DIRECTION ( 'NONE',  ( 0.000000000000000000, 0.000000000000000000, 1.000000000000000000 ) ) ;
#4812 = CIRCLE ( 'NONE', #8552, 2.500000000000002220 ) ;
#4811 = CARTESIAN_POINT ( 'NONE',  ( -3.999999999999990674, -1.658477411507763621, -3.231534348143921598 ) ) ;
#4813 = CARTESIAN_POINT ( 'NONE',  ( 20.00000000000000000, 60.00000000000000711, -25.00000000000000000 ) ) ;
#4814 = CARTESIAN_POINT ( 'NONE',  ( -3.333333333333330817, 2.694301256218247342, -3.000726591567076440 ) ) ;
#4815 = EDGE_LOOP ( 'NONE', ( #9474, #2568, #477, #646 ) ) ;
#4816 = DIRECTION ( 'NONE',  ( 0.000000000000000000, 0.000000000000000000, -1.000000000000000000 ) ) ;
#4817 = EDGE_LOOP ( 'NONE', ( #12123, #8622, #3426, #7107 ) ) ;
#4818 = LINE ( 'NONE', #7074, #12605 ) ;
#4819 = DIRECTION ( 'NONE',  ( 0.000000000000000000, 1.000000000000000000, 0.000000000000000000 ) ) ;
#4820 = CARTESIAN_POINT ( 'NONE',  ( 20.00000000000000000, 70.00000000000000000, -25.00000000000000000 ) ) ;
#4821 = CARTESIAN_POINT ( 'NONE',  ( 30.07694101601105530, 130.0000000000000000, 25.00000000000000000 ) ) ;
#4822 = CARTESIAN_POINT ( 'NONE',  ( -118.6817075744281595, 69.57655509336025546, 0.000000000000000000 ) ) ;
#4823 = CARTESIAN_POINT ( 'NONE',  ( -25.00000000000000000, 199.5765550933606107, 47.99999999999998579 ) ) ;
#4824 = DIRECTION ( 'NONE',  ( 1.000000000000000000, 0.000000000000000000, 0.000000000000000000 ) ) ;
#4825 = CARTESIAN_POINT ( 'NONE',  ( 22.00000000000000355, 47.00000000000000000, 25.00000000000000000 ) ) ;
#4826 = DIRECTION ( 'NONE',  ( -1.913084959030911013E-15, 1.000000000000000000, 0.000000000000000000 ) ) ;
#4827 = ORIENTED_EDGE ( 'NONE', *, *, #1236, .F. ) ;
#4828 = DIRECTION ( 'NONE',  ( 1.000000000000000000, 0.000000000000000000, 0.000000000000000000 ) ) ;
#4829 = ORIENTED_EDGE ( 'NONE', *, *, #11688, .F. ) ;
#4830 = VERTEX_POINT ( 'NONE', #11008 ) ;
#4831 = VECTOR ( 'NONE', #11737, 1000.000000000000000 ) ;
#4832 = EDGE_LOOP ( 'NONE', ( #9169, #12336, #14242, #4068 ) ) ;
#4833 = ORIENTED_EDGE ( 'NONE', *, *, #4873, .F. ) ;
#4834 = EDGE_CURVE ( 'NONE', #937, #4572, #4015, .T. ) ;
#4835 = CARTESIAN_POINT ( 'NONE',  ( 37.35300976710104948, 100.8957249956400375, 25.00000000000000000 ) ) ;
#4836 = FACE_OUTER_BOUND ( 'NONE', #2007, .T. ) ;
#4837 = EDGE_LOOP ( 'NONE', ( #1430, #7776, #7577, #3372 ) ) ;
#4838 = ORIENTED_EDGE ( 'NONE', *, *, #12526, .T. ) ;
#4839 = CARTESIAN_POINT ( 'NONE',  ( 60.00000000000000000, -6.123233995736768255E-16, 25.00000000000000000 ) ) ;
#4840 = CIRCLE ( 'NONE', #10693, 2.500000000000009326 ) ;
#4841 = DIRECTION ( 'NONE',  ( -1.892425610156517368E-16, -1.000000000000000000, 0.000000000000000000 ) ) ;
#4842 = VERTEX_POINT ( 'NONE', #5451 ) ;
#4843 = EDGE_CURVE ( 'NONE', #904, #8755, #6404, .T. ) ;
#4844 = DIRECTION ( 'NONE',  ( -1.000000000000000000, 2.551526159633733968E-19, 1.987661601597216239E-18 ) ) ;
#4845 = ORIENTED_EDGE ( 'NONE', *, *, #14443, .T. ) ;
#4846 = UNCERTAINTY_MEASURE_WITH_UNIT (LENGTH_MEASURE( 1.000000000000000082E-05 ), #6032, 'distance_accuracy_value', 'NONE');
#4847 = EDGE_CURVE ( 'NONE', #13538, #1393, #985, .T. ) ;
#4848 = CARTESIAN_POINT ( 'NONE',  ( 0.2494252716045076701, 1.935831255945836604, -4.000000000000003553 ) ) ;
#4849 = CARTESIAN_POINT ( 'NONE',  ( 51.97979101891770171, 52.38859998837343568, 25.00000000000000000 ) ) ;
#4850 = CIRCLE ( 'NONE', #1116, 3.299999999999969624 ) ;
#4851 = AXIS2_PLACEMENT_3D ( 'NONE', #10890, #6483, #10959 ) ;
#4852 = FACE_OUTER_BOUND ( 'NONE', #3049, .T. ) ;
#4853 = DIRECTION ( 'NONE',  ( 0.9701425001453318764, 0.2425356250363329969, 0.000000000000000000 ) ) ;
#4854 =( LENGTH_UNIT ( ) NAMED_UNIT ( * ) SI_UNIT ( .MILLI., .METRE. ) );
#4855 = CARTESIAN_POINT ( 'NONE',  ( 1.721886139900248969, 5.052888355619074900, -4.357689166958493843 ) ) ;
#4856 = DIRECTION ( 'NONE',  ( -1.000000000000000000, 0.000000000000000000, 0.000000000000000000 ) ) ;
#4857 = ORIENTED_EDGE ( 'NONE', *, *, #6320, .T. ) ;
#4858 = FACE_OUTER_BOUND ( 'NONE', #8203, .T. ) ;
#4859 = CARTESIAN_POINT ( 'NONE',  ( 20.00000000000000355, 30.00000000000000711, 25.00000000000000000 ) ) ;
#4860 = DIRECTION ( 'NONE',  ( -1.000000000000000000, -0.000000000000000000, -0.000000000000000000 ) ) ;
#4861 = VERTEX_POINT ( 'NONE', #2787 ) ;
#4862 = CARTESIAN_POINT ( 'NONE',  ( 4.847001880572340049, -3.049720480807998513, -2.717729178357026321 ) ) ;
#4863 = AXIS2_PLACEMENT_3D ( 'NONE', #8120, #6824, #5705 ) ;
#4864 = EDGE_CURVE ( 'NONE', #10880, #12702, #512, .T. ) ;
#4865 = AXIS2_PLACEMENT_3D ( 'NONE', #13089, #846, #13164 ) ;
#4866 = ORIENTED_EDGE ( 'NONE', *, *, #3418, .T. ) ;
#4867 = CIRCLE ( 'NONE', #2789, 2.749999999999997780 ) ;
#4868 = CARTESIAN_POINT ( 'NONE',  ( 5.000882498481359129, 4.618802153517016507, 1.397365476814232024E-14 ) ) ;
#4869 = ORIENTED_EDGE ( 'NONE', *, *, #14344, .F. ) ;
#4870 = ORIENTED_EDGE ( 'NONE', *, *, #1088, .F. ) ;
#4871 = PLANE ( 'NONE',  #5244 ) ;
#4872 = CARTESIAN_POINT ( 'NONE',  ( 5.000000000000001776, 2.886751345948120662, -4.284345921091780696 ) ) ;
#4873 = EDGE_CURVE ( 'NONE', #14315, #661, #422, .T. ) ;
#4874 = ADVANCED_FACE ( 'NONE', ( #4234 ), #14221, .F. ) ;
#4875 = DIRECTION ( 'NONE',  ( 0.3822382184081047352, -0.9240638205168505426, -0.000000000000000000 ) ) ;
#4876 = DIRECTION ( 'NONE',  ( -1.000000000000000000, 0.000000000000000000, 0.000000000000000000 ) ) ;
#4877 = CYLINDRICAL_SURFACE ( 'NONE', #1595, 2.500000000000002220 ) ;
#4878 = VECTOR ( 'NONE', #2467, 1000.000000000000000 ) ;
#4879 = CARTESIAN_POINT ( 'NONE',  ( 92.68170757442806007, 124.5765550933605965, -25.00000000000000000 ) ) ;
#4880 = CARTESIAN_POINT ( 'NONE',  ( 2.499999999999997780, -4.330127018922222959, -3.920524600599856413 ) ) ;
#4881 = CARTESIAN_POINT ( 'NONE',  ( 62.10586122665987574, -20.42344490663940704, 28.00000000000000000 ) ) ;
#4882 = CARTESIAN_POINT ( 'NONE',  ( 22.00000000000000355, 30.00000000000000711, 25.00000000000000000 ) ) ;
#4883 = EDGE_CURVE ( 'NONE', #1693, #5595, #178, .T. ) ;
#4884 = ORIENTED_EDGE ( 'NONE', *, *, #6439, .T. ) ;
#4885 = EDGE_LOOP ( 'NONE', ( #5301, #1513 ) ) ;
#4886 = VECTOR ( 'NONE', #7078, 1000.000000000000114 ) ;
#4887 = LINE ( 'NONE', #505, #9672 ) ;
#4888 = ORIENTED_EDGE ( 'NONE', *, *, #14076, .F. ) ;
#4889 = ORIENTED_EDGE ( 'NONE', *, *, #12459, .T. ) ;
#4890 = LINE ( 'NONE', #11619, #13113 ) ;
#4891 = AXIS2_PLACEMENT_3D ( 'NONE', #4116, #12643, #1529 ) ;
#4892 = DIRECTION ( 'NONE',  ( 0.000000000000000000, 0.000000000000000000, -1.000000000000000000 ) ) ;
#4893 = LINE ( 'NONE', #2634, #13314 ) ;
#4894 = DIRECTION ( 'NONE',  ( 1.000000000000000000, 0.000000000000000000, 0.000000000000000000 ) ) ;
#4895 = LINE ( 'NONE', #8254, #11957 ) ;
#4896 = CARTESIAN_POINT ( 'NONE',  ( -2.696105871110437585E-15, -0.3420925509381240182, 3.499999999999996891 ) ) ;
#4897 = CARTESIAN_POINT ( 'NONE',  ( 5.103531824934115946, 2.354098498486452584, 4.077418205400126894 ) ) ;
#4898 = DIRECTION ( 'NONE',  ( -0.9701425001453318764, -0.2425356250363329969, 0.000000000000000000 ) ) ;
#4899 = AXIS2_PLACEMENT_3D ( 'NONE', #13981, #3884, #5703 ) ;
#4900 = EDGE_CURVE ( 'NONE', #7164, #3184, #13997, .T. ) ;
#4901 = ADVANCED_FACE ( 'NONE', ( #11302 ), #2305, .T. ) ;
#4902 = FACE_OUTER_BOUND ( 'NONE', #11077, .T. ) ;
#4903 = ORIENTED_EDGE ( 'NONE', *, *, #4547, .T. ) ;
#4904 = VERTEX_POINT ( 'NONE', #8880 ) ;
#4905 = EDGE_LOOP ( 'NONE', ( #8003, #13256, #10, #7280 ) ) ;
#4906 = EDGE_CURVE ( 'NONE', #2047, #2270, #7649, .T. ) ;
#4907 = AXIS2_PLACEMENT_3D ( 'NONE', #7338, #5360, #1790 ) ;
#4908 = CARTESIAN_POINT ( 'NONE',  ( 4.000000000000000000, 6.661338147750937270E-16, 1.599999999999990319 ) ) ;
#4909 = CARTESIAN_POINT ( 'NONE',  ( -4.211140560182201398, -2.431303136016548017, -3.445885042887453231 ) ) ;
#4910 =( NAMED_UNIT ( * ) PLANE_ANGLE_UNIT ( ) SI_UNIT ( $, .RADIAN. ) );
#4911 = VERTEX_POINT ( 'NONE', #7995 ) ;
#4912 = EDGE_LOOP ( 'NONE', ( #1695, #9906, #9590, #6566 ) ) ;
#4913 = DIRECTION ( 'NONE',  ( 0.000000000000000000, 1.000000000000000000, 0.000000000000000000 ) ) ;
#4914 = AXIS2_PLACEMENT_3D ( 'NONE', #4606, #7947, #2695 ) ;
#4915 = DIRECTION ( 'NONE',  ( -0.9701425001453319874, -0.2425356250363330801, 0.000000000000000000 ) ) ;
#4916 = AXIS2_PLACEMENT_3D ( 'NONE', #12490, #13892, #13821 ) ;
#4917 = ORIENTED_EDGE ( 'NONE', *, *, #4684, .F. ) ;
#4918 = CARTESIAN_POINT ( 'NONE',  ( 21.68170757442799967, 141.2731697022880155, -28.00000000000000000 ) ) ;
#4919 = CIRCLE ( 'NONE', #7474, 3.499999999999999112 ) ;
#4920 = B_SPLINE_CURVE_WITH_KNOTS ( 'NONE', 3,
 ( #3716, #11600, #10510, #4949, #842, #4162, #5242, #12945, #14248, #14043, #1879, #13161, #13959, #9632, #10805, #9769 ),
 .UNSPECIFIED., .F., .F.,
 ( 4, 3, 3, 3, 3, 4 ),
 ( 0.000000000000000000, 3.647308126642952050E-05, 7.269606878413157171E-05, 0.0001129253843484943226, 0.0001515766232005118122, 0.0001537911822990430675 ),
 .UNSPECIFIED. ) ;
#4921 = B_SPLINE_CURVE_WITH_KNOTS ( 'NONE', 3,
 ( #14223, #4205, #12026, #8643, #13133, #3458 ),
 .UNSPECIFIED., .F., .F.,
 ( 4, 2, 4 ),
 ( -3.988673288090718192E-06, 0.0002483701411510679750, 0.0005007289555902266114 ),
 .UNSPECIFIED. ) ;
#4922 = CARTESIAN_POINT ( 'NONE',  ( -1.747541505913280391, 3.837784562140261535, -3.203702292528891604 ) ) ;
#4923 = DIRECTION ( 'NONE',  ( 0.000000000000000000, 1.000000000000000000, 0.000000000000000000 ) ) ;
#4924 = ORIENTED_EDGE ( 'NONE', *, *, #5928, .T. ) ;
#4925 = CIRCLE ( 'NONE', #14290, 5.315148208181398104 ) ;
#4926 = CARTESIAN_POINT ( 'NONE',  ( -5.236872748402763733, 0.5081686017868803917, -4.357689166958460980 ) ) ;
#4927 = AXIS2_PLACEMENT_3D ( 'NONE', #14166, #8365, #6316 ) ;
#4928 = CARTESIAN_POINT ( 'NONE',  ( 0.000000000000000000, 0.000000000000000000, 0.000000000000000000 ) ) ;
#4929 = DIRECTION ( 'NONE',  ( 0.000000000000000000, 0.000000000000000000, -1.000000000000000000 ) ) ;
#4930 = ADVANCED_FACE ( 'NONE', ( #2240, #14393 ), #1133, .T. ) ;
#4931 = DIRECTION ( 'NONE',  ( 1.000000000000000000, 0.000000000000000000, 0.000000000000000000 ) ) ;
#4932 = VECTOR ( 'NONE', #14440, 1000.000000000000000 ) ;
#4933 = ORIENTED_EDGE ( 'NONE', *, *, #2729, .T. ) ;
#4934 = CARTESIAN_POINT ( 'NONE',  ( 21.68170757442799967, 141.2731697022880155, -32.99999999999999289 ) ) ;
#4935 = DIRECTION ( 'NONE',  ( 0.000000000000000000, 0.000000000000000000, 1.000000000000000000 ) ) ;
#4936 = EDGE_CURVE ( 'NONE', #11358, #6890, #5585, .T. ) ;
#4937 = ORIENTED_EDGE ( 'NONE', *, *, #11603, .F. ) ;
#4938 = CARTESIAN_POINT ( 'NONE',  ( 6.800000000000028244, 4.898485791573355875E-15, -6.250000000000000000 ) ) ;
#4939 = EDGE_CURVE ( 'NONE', #6876, #14018, #3417, .T. ) ;
#4940 = AXIS2_PLACEMENT_3D ( 'NONE', #10891, #1760, #10753 ) ;
#4941 = CARTESIAN_POINT ( 'NONE',  ( 5.108576461337683838, 2.340462348500683021, 4.101226464158124863 ) ) ;
#4942 = VECTOR ( 'NONE', #4624, 1000.000000000000000 ) ;
#4943 = LINE ( 'NONE', #5949, #11951 ) ;
#4944 = VERTEX_POINT ( 'NONE', #5785 ) ;
#4945 = ORIENTED_EDGE ( 'NONE', *, *, #3172, .F. ) ;
#4946 = FACE_OUTER_BOUND ( 'NONE', #6715, .T. ) ;
#4947 = DIRECTION ( 'NONE',  ( 1.000000000000000000, 0.000000000000000000, 0.000000000000000000 ) ) ;
#4948 = ORIENTED_EDGE ( 'NONE', *, *, #773, .F. ) ;
#4949 = CARTESIAN_POINT ( 'NONE',  ( 5.024612689793206854, -2.312654742478263525, 4.005635514337482661 ) ) ;
#4950 = CARTESIAN_POINT ( 'NONE',  ( 105.6817075744281311, 124.5765550933606107, -25.00000000000000000 ) ) ;
#4951 = AXIS2_PLACEMENT_3D ( 'NONE', #10869, #8532, #3060 ) ;
#4952 = CARTESIAN_POINT ( 'NONE',  ( 105.6817075744281311, 124.5765550933606107, 25.00000000000000000 ) ) ;
#4953 = EDGE_CURVE ( 'NONE', #13868, #9429, #7712, .T. ) ;
#4954 = AXIS2_PLACEMENT_3D ( 'NONE', #13901, #12782, #1298 ) ;
#4955 = AXIS2_PLACEMENT_3D ( 'NONE', #13724, #9243, #2592 ) ;
#4956 = FACE_OUTER_BOUND ( 'NONE', #13251, .T. ) ;
#4957 = DIRECTION ( 'NONE',  ( 0.000000000000000000, 0.000000000000000000, 1.000000000000000000 ) ) ;
#4958 = DIRECTION ( 'NONE',  ( 0.000000000000000000, -8.482162385747133845E-47, 1.000000000000000000 ) ) ;
#4959 = PLANE ( 'NONE',  #4954 ) ;
#4960 = DIRECTION ( 'NONE',  ( 1.000000000000000000, 1.665334536937734071E-16, 0.000000000000000000 ) ) ;
#4961 = SHAPE_REPRESENTATION ( 'hex flange nut gradea_iso_ISO - 4161 - M6 - N', ( #11025 ), #5842 ) ;
#4962 = AXIS2_PLACEMENT_3D ( 'NONE', #5912, #10394, #372 ) ;
#4963 = ORIENTED_EDGE ( 'NONE', *, *, #8310, .T. ) ;
#4964 = CARTESIAN_POINT ( 'NONE',  ( 139.9999999999996874, 189.5765550933606107, 47.99999999999998579 ) ) ;
#4965 = ORIENTED_EDGE ( 'NONE', *, *, #5036, .F. ) ;
#4966 = VERTEX_POINT ( 'NONE', #13582 ) ;
#4967 = LINE ( 'NONE', #9281, #7699 ) ;
#4968 = CARTESIAN_POINT ( 'NONE',  ( -88.22284556172398595, 39.57655509336048283, -117.0000000000000000 ) ) ;
#4969 = DIRECTION ( 'NONE',  ( -1.000000000000000000, 0.000000000000000000, 0.000000000000000000 ) ) ;
#4970 = FACE_OUTER_BOUND ( 'NONE', #384, .T. ) ;
#4971 = EDGE_CURVE ( 'NONE', #5200, #2033, #7852, .T. ) ;
#4972 = FACE_OUTER_BOUND ( 'NONE', #5039, .T. ) ;
#4973 = CARTESIAN_POINT ( 'NONE',  ( -2.500000000000002220, -4.163336342344338999E-16, -4.674599999999973221 ) ) ;
#4974 = DIRECTION ( 'NONE',  ( -4.664070103548418288E-16, -0.9242245927363028635, -0.3818493186865930533 ) ) ;
#4975 = DIRECTION ( 'NONE',  ( -1.000000000000000000, 0.000000000000000000, -0.000000000000000000 ) ) ;
#4976 = DIRECTION ( 'NONE',  ( 2.133709875451472726E-16, -1.000000000000000000, -0.000000000000000000 ) ) ;
#4977 = AXIS2_PLACEMENT_3D ( 'NONE', #5710, #5646, #4445 ) ;
#4978 = PRODUCT_DEFINITION_SHAPE ( 'NONE', 'NONE',  #13230 ) ;
#4979 = EDGE_CURVE ( 'NONE', #1693, #6358, #14391, .T. ) ;
#4980 = DIRECTION ( 'NONE',  ( 0.3420201433256618850, -4.173946208010309292E-16, -0.9396926207859108704 ) ) ;
#4981 = ORIENTED_EDGE ( 'NONE', *, *, #12899, .F. ) ;
#4982 = ORIENTED_EDGE ( 'NONE', *, *, #13259, .F. ) ;
#4983 = EDGE_LOOP ( 'NONE', ( #7915, #10383, #9231, #8076 ) ) ;
#4984 = AXIS2_PLACEMENT_3D ( 'NONE', #5856, #5933, #12751 ) ;
#4985 = ORIENTED_EDGE ( 'NONE', *, *, #205, .T. ) ;
#4986 = VECTOR ( 'NONE', #12027, 1000.000000000000000 ) ;
#4987 = DIRECTION ( 'NONE',  ( 0.000000000000000000, 1.000000000000000000, 0.000000000000000000 ) ) ;
#4988 = CARTESIAN_POINT ( 'NONE',  ( 58.68170757442803165, 29.57655509336062849, 27.99999999999999645 ) ) ;
#4989 = EDGE_CURVE ( 'NONE', #2424, #13364, #1827, .T. ) ;
#4990 = PRODUCT_DEFINITION ( 'UNKNOWN', '', #9904, #13349 ) ;
#4991 = EDGE_CURVE ( 'NONE', #549, #7236, #1770, .T. ) ;
#4993 = AXIS2_PLACEMENT_3D ( 'NONE', #4964, #11777, #12634 ) ;
#4992 =( LENGTH_UNIT ( ) NAMED_UNIT ( * ) SI_UNIT ( .MILLI., .METRE. ) );
#4994 = VERTEX_POINT ( 'NONE', #13445 ) ;
#4995 = ITEM_DEFINED_TRANSFORMATION ( 'NONE', 'NONE', #3604,  #11025 ) ;
#4996 = VERTEX_POINT ( 'NONE', #6754 ) ;
#4997 = CARTESIAN_POINT ( 'NONE',  ( 20.00000000000000000, 78.00000000000000000, 25.00000000000000000 ) ) ;
#4998 = LINE ( 'NONE', #4778, #11028 ) ;
#4999 = EDGE_LOOP ( 'NONE', ( #11377, #3935, #5398, #1946 ) ) ;
#5000 = CARTESIAN_POINT ( 'NONE',  ( 62.10586122665984732, -20.42344490663941414, -23.00000000000000000 ) ) ;
#5001 = AXIS2_PLACEMENT_3D ( 'NONE', #569, #2607, #10658 ) ;
#5002 = ORIENTED_EDGE ( 'NONE', *, *, #9870, .F. ) ;
#5003 = UNCERTAINTY_MEASURE_WITH_UNIT (LENGTH_MEASURE( 1.000000000000000082E-05 ), #13584, 'distance_accuracy_value', 'NONE');
#5004 = CARTESIAN_POINT ( 'NONE',  ( -0.3461262719736090121, 4.658553426539293163, -3.371615880910392438 ) ) ;
#5005 = DIRECTION ( 'NONE',  ( 0.2425356250363328581, -0.9701425001453318764, 0.000000000000000000 ) ) ;
#5006 = COLOUR_RGB ( '', 0.31764706, 0.68627451, 0.89019608) ;
#5007 = CYLINDRICAL_SURFACE ( 'NONE', #6448, 9.000000000000001776 ) ;
#5008 = ORIENTED_EDGE ( 'NONE', *, *, #13645, .T. ) ;
#5009 = CARTESIAN_POINT ( 'NONE',  ( 28.00000000000000355, 29.99999999999999645, -34.50000000000000000 ) ) ;
#5010 = CARTESIAN_POINT ( 'NONE',  ( 59.10586122665984732, -20.42344490663941414, -23.00000000000000000 ) ) ;
#5011 = ORIENTED_EDGE ( 'NONE', *, *, #14287, .F. ) ;
#5012 = DIRECTION ( 'NONE',  ( 0.000000000000000000, 0.000000000000000000, 1.000000000000000000 ) ) ;
#5013 = CYLINDRICAL_SURFACE ( 'NONE', #1214, 2.100000000000000977 ) ;
#5014 = VERTEX_POINT ( 'NONE', #11224 ) ;
#5015 = CARTESIAN_POINT ( 'NONE',  ( 1.642566673137918487, 4.825166380998191507, -0.07080520455422339987 ) ) ;
#5016 = CARTESIAN_POINT ( 'NONE',  ( 3.453019673806204004, 2.625200315326535971, -3.235259548910409677 ) ) ;
#5017 = EDGE_LOOP ( 'NONE', ( #10657, #2045, #12635, #9101 ) ) ;
#5018 = CARTESIAN_POINT ( 'NONE',  ( 79.68170757442804586, 124.5765550933606249, 25.00000000000000000 ) ) ;
#5019 = FACE_BOUND ( 'NONE', #3790, .T. ) ;
#5020 = CARTESIAN_POINT ( 'NONE',  ( 5.091953023115830312, 4.682427078960528455, -1.387060565653463815E-14 ) ) ;
#5021 = ORIENTED_EDGE ( 'NONE', *, *, #5248, .F. ) ;
#5022 = VERTEX_POINT ( 'NONE', #2378 ) ;
#5023 = CARTESIAN_POINT ( 'NONE',  ( 108.6817075744280743, 29.57655509336062849, -106.9999999999999858 ) ) ;
#5024 = CARTESIAN_POINT ( 'NONE',  ( -13.00000000000000533, 29.99999999999999289, 8.000000000000007105 ) ) ;
#5025 = VERTEX_POINT ( 'NONE', #1205 ) ;
#5026 = LINE ( 'NONE', #5170, #1183 ) ;
#5027 = EDGE_CURVE ( 'NONE', #8393, #11633, #3638, .T. ) ;
#5028 = PLANE ( 'NONE',  #3453 ) ;
#5029 = CARTESIAN_POINT ( 'NONE',  ( 20.00000000000000000, -5.510910596163090344E-15, 25.00000000000000000 ) ) ;
#5030 = DIRECTION ( 'NONE',  ( -1.000000000000000000, 0.000000000000000000, 0.000000000000000000 ) ) ;
#5031 =( LENGTH_UNIT ( ) NAMED_UNIT ( * ) SI_UNIT ( .MILLI., .METRE. ) );
#5032 = LINE ( 'NONE', #13827, #6791 ) ;
#5033 = DIRECTION ( 'NONE',  ( 1.000000000000000000, 0.000000000000000000, 0.000000000000000000 ) ) ;
#5034 = CARTESIAN_POINT ( 'NONE',  ( 22.00000000000000000, 60.00000000000000711, -25.00000000000000000 ) ) ;
#5035 = DIRECTION ( 'NONE',  ( -0.000000000000000000, 1.000000000000000000, -0.000000000000000000 ) ) ;
#5036 = EDGE_CURVE ( 'NONE', #2687, #2858, #4587, .T. ) ;
#5037 = EDGE_LOOP ( 'NONE', ( #741, #3661, #11875, #1311 ) ) ;
#5038 = LINE ( 'NONE', #2859, #4762 ) ;
#5039 = EDGE_LOOP ( 'NONE', ( #12919, #12389, #8672, #10239, #10737 ) ) ;
#5040 = VERTEX_POINT ( 'NONE', #7925 ) ;
#5041 = LINE ( 'NONE', #6346, #6303 ) ;
#5042 = ADVANCED_FACE ( 'NONE', ( #12399 ), #2710, .T. ) ;
#5043 = DIRECTION ( 'NONE',  ( 0.000000000000000000, 0.000000000000000000, -1.000000000000000000 ) ) ;
#5044 = DIRECTION ( 'NONE',  ( -0.000000000000000000, -1.000000000000000000, -0.000000000000000000 ) ) ;
#5045 = CARTESIAN_POINT ( 'NONE',  ( -118.6817075744279606, -30.42344490663958112, -117.0000000000000000 ) ) ;
#5046 = AXIS2_PLACEMENT_3D ( 'NONE', #7159, #3895, #12983 ) ;
#5047 = LINE ( 'NONE', #9355, #7258 ) ;
#5048 = CARTESIAN_POINT ( 'NONE',  ( 22.00000000000000711, 20.00000000000000355, -25.00000000000000000 ) ) ;
#5049 = FACE_OUTER_BOUND ( 'NONE', #10526, .T. ) ;
#5050 = CARTESIAN_POINT ( 'NONE',  ( 2.949999999999994404, 0.000000000000000000, 2.499999999999999112 ) ) ;
#5051 = CARTESIAN_POINT ( 'NONE',  ( 5.599999999999994316, 0.000000000000000000, 0.000000000000000000 ) ) ;
#5052 = ADVANCED_FACE ( 'NONE', ( #11433 ), #7261, .T. ) ;
#5053 = ORIENTED_EDGE ( 'NONE', *, *, #1983, .F. ) ;
#5054 = VERTEX_POINT ( 'NONE', #470 ) ;
#5055 = DIRECTION ( 'NONE',  ( -0.000000000000000000, -0.000000000000000000, -1.000000000000000000 ) ) ;
#5056 = PLANE ( 'NONE',  #3278 ) ;
#5057 = VERTEX_POINT ( 'NONE', #13873 ) ;
#5058 = CARTESIAN_POINT ( 'NONE',  ( 0.000000000000000000, 1.732050807568871864, 0.000000000000000000 ) ) ;
#5059 = DIRECTION ( 'NONE',  ( -1.000000000000000000, 0.000000000000000000, 0.000000000000000000 ) ) ;
#5060 = VECTOR ( 'NONE', #1047, 1000.000000000000000 ) ;
#5061 = ORIENTED_EDGE ( 'NONE', *, *, #2541, .T. ) ;
#5062 = EDGE_CURVE ( 'NONE', #13646, #7747, #13796, .T. ) ;
#5063 = DIRECTION ( 'NONE',  ( -0.2425356250363328581, 0.9701425001453318764, 0.000000000000000000 ) ) ;
#5064 = VERTEX_POINT ( 'NONE', #1557 ) ;
#5065 = DIRECTION ( 'NONE',  ( -0.5000000000000024425, 0.8660254037844373753, 8.404057939144334946E-32 ) ) ;
#5066 = LINE ( 'NONE', #6441, #8059 ) ;
#5067 = CARTESIAN_POINT ( 'NONE',  ( 71.80728622811317052, -17.99808865627607801, 25.00000000000000000 ) ) ;
#5068 = VERTEX_POINT ( 'NONE', #5010 ) ;
#5069 = CARTESIAN_POINT ( 'NONE',  ( -3.081487911019577365E-30, 3.469446951953614189E-15, -5.974599999999997024 ) ) ;
#5070 = CARTESIAN_POINT ( 'NONE',  ( 62.10586122665984732, -20.42344490663941414, -35.00000000000000000 ) ) ;
#5071 = ORIENTED_EDGE ( 'NONE', *, *, #14458, .T. ) ;
#5072 = CARTESIAN_POINT ( 'NONE',  ( 1.598077599629971202, 4.850852159564532862, -4.271474537231044089 ) ) ;
#5073 = DIRECTION ( 'NONE',  ( -0.9396926207859143121, 2.901070394884691809E-47, -0.3420201433256522816 ) ) ;
#5074 = ORIENTED_EDGE ( 'NONE', *, *, #2541, .F. ) ;
#5075 = LINE ( 'NONE', #11744, #6794 ) ;
#5076 = LINE ( 'NONE', #9551, #3262 ) ;
#5077 = DIRECTION ( 'NONE',  ( 0.000000000000000000, -8.482162385747133845E-47, 1.000000000000000000 ) ) ;
#5078 = EDGE_LOOP ( 'NONE', ( #1823, #2960, #13006, #5011 ) ) ;
#5079 = LINE ( 'NONE', #10794, #11376 ) ;
#5080 = EDGE_CURVE ( 'NONE', #12535, #3564, #3764, .T. ) ;
#5081 = FACE_BOUND ( 'NONE', #6073, .T. ) ;
#5082 = ADVANCED_FACE ( 'NONE', ( #3912 ), #8061, .T. ) ;
#5083 = VECTOR ( 'NONE', #11824, 1000.000000000000000 ) ;
#5084 = CARTESIAN_POINT ( 'NONE',  ( 5.103021810857300444, 4.706811482981981598, -7.866781916910138702E-14 ) ) ;
#5085 = ORIENTED_EDGE ( 'NONE', *, *, #4565, .F. ) ;
#5086 = CIRCLE ( 'NONE', #5763, 3.000000000000001332 ) ;
#5087 = ORIENTED_EDGE ( 'NONE', *, *, #3091, .T. ) ;
#5088 = DIRECTION ( 'NONE',  ( 0.000000000000000000, 0.000000000000000000, -1.000000000000000000 ) ) ;
#5089 = DIRECTION ( 'NONE',  ( 0.000000000000000000, 0.000000000000000000, 1.000000000000000000 ) ) ;
#5090 = EDGE_LOOP ( 'NONE', ( #2347, #10091, #723 ) ) ;
#5091 = DIRECTION ( 'NONE',  ( 1.000000000000000000, 1.723842398015259277E-15, -0.000000000000000000 ) ) ;
#5092 = CARTESIAN_POINT ( 'NONE',  ( 5.560781378645576645, 1.607055439833521515E-15, -3.699999999999981082 ) ) ;
#5093 = DIRECTION ( 'NONE',  ( 0.000000000000000000, 0.000000000000000000, 1.000000000000000000 ) ) ;
#5094 = CARTESIAN_POINT ( 'NONE',  ( 4.175813232069169878, -2.061359961916364725, 3.570380186727409200 ) ) ;
#5095 = ORIENTED_EDGE ( 'NONE', *, *, #11919, .T. ) ;
#5096 = VECTOR ( 'NONE', #6587, 1000.000000000000000 ) ;
#5097 = DIRECTION ( 'NONE',  ( -0.9701425001453319874, -0.2425356250363328858, 0.000000000000000000 ) ) ;
#5098 = VECTOR ( 'NONE', #6261, 1000.000000000000000 ) ;
#5099 = CARTESIAN_POINT ( 'NONE',  ( 3.567687560464438246, -3.713697318477663600, -0.1121614189353530300 ) ) ;
#5100 = EDGE_CURVE ( 'NONE', #13268, #4944, #11818, .T. ) ;
#5101 = EDGE_CURVE ( 'NONE', #5665, #12241, #4718, .T. ) ;
#5102 = VERTEX_POINT ( 'NONE', #1716 ) ;
#5103 = CYLINDRICAL_SURFACE ( 'NONE', #11069, 5.000000000000004441 ) ;
#5104 = ORIENTED_EDGE ( 'NONE', *, *, #2376, .T. ) ;
#5105 = EDGE_CURVE ( 'NONE', #6397, #9797, #1589, .T. ) ;
#5106 = EDGE_LOOP ( 'NONE', ( #11663, #6184, #10149, #7042, #11543, #2299, #7476, #9228 ) ) ;
#5107 = CIRCLE ( 'NONE', #9558, 3.299999999999983391 ) ;
#5108 = LINE ( 'NONE', #4031, #3512 ) ;
#5109 = CARTESIAN_POINT ( 'NONE',  ( 0.000000000000000000, 1.387778780781445676E-14, 3.499999999999982236 ) ) ;
#5110 = DIRECTION ( 'NONE',  ( 0.000000000000000000, 0.000000000000000000, -1.000000000000000000 ) ) ;
#5111 = DIRECTION ( 'NONE',  ( 2.960064101202773706E-17, 0.8660254037844384856, 0.5000000000000004441 ) ) ;
#5112 = DIRECTION ( 'NONE',  ( -1.000000000000000000, 0.000000000000000000, 1.276920294826117846E-16 ) ) ;
#5113 = APPLICATION_PROTOCOL_DEFINITION ( 'draft international standard', 'automotive_design', 1998, #9027 ) ;
#5114 = DIRECTION ( 'NONE',  ( -1.000000000000000000, 0.000000000000000000, 0.000000000000000000 ) ) ;
#5115 = APPLICATION_CONTEXT ( 'automotive_design' ) ;
#5116 = ADVANCED_FACE ( 'NONE', ( #9390 ), #324, .F. ) ;
#5117 = DIRECTION ( 'NONE',  ( 0.000000000000000000, 0.000000000000000000, -1.000000000000000000 ) ) ;
#5118 = CIRCLE ( 'NONE', #208, 6.250000000000007105 ) ;
#5119 = CARTESIAN_POINT ( 'NONE',  ( 18.68170757442808849, 141.2731697022877313, -35.00000000000000000 ) ) ;
#5120 = ADVANCED_FACE ( 'NONE', ( #4787 ), #3021, .T. ) ;
#5121 = ORIENTED_EDGE ( 'NONE', *, *, #7478, .F. ) ;
#5122 = EDGE_CURVE ( 'NONE', #47, #6994, #1124, .T. ) ;
#5123 = ORIENTED_EDGE ( 'NONE', *, *, #1819, .T. ) ;
#5124 = ORIENTED_EDGE ( 'NONE', *, *, #9852, .T. ) ;
#5125 = CARTESIAN_POINT ( 'NONE',  ( 0.3572655899082288755, 4.618802153517023612, 1.387778780781445676E-14 ) ) ;
#5126 = CARTESIAN_POINT ( 'NONE',  ( 6.800000000000028244, -4.163336342344337027E-15, 6.250000000000007105 ) ) ;
#5127 = AXIS2_PLACEMENT_3D ( 'NONE', #12797, #7307, #12645 ) ;
#5128 = ADVANCED_FACE ( 'NONE', ( #8210 ), #10636, .T. ) ;
#5129 = ADVANCED_FACE ( 'NONE', ( #12754, #2741, #13662, #12679, #7183, #11657 ), #7036, .F. ) ;
#5130 = ORIENTED_EDGE ( 'NONE', *, *, #11187, .T. ) ;
#5131 = AXIS2_PLACEMENT_3D ( 'NONE', #10472, #453, #10548 ) ;
#5132 = ORIENTED_EDGE ( 'NONE', *, *, #2515, .T. ) ;
#5133 = B_SPLINE_CURVE_WITH_KNOTS ( 'NONE', 3,
 ( #3595, #13627, #12506, #5820 ),
 .UNSPECIFIED., .F., .F.,
 ( 4, 4 ),
 ( 0.002376763279741518631, 0.004766460739942336711 ),
 .UNSPECIFIED. ) ;
#5134 = LINE ( 'NONE', #7327, #9301 ) ;
#5135 = DIRECTION ( 'NONE',  ( -0.2425356250363330801, 0.9701425001453319874, 0.000000000000000000 ) ) ;
#5136 = EDGE_LOOP ( 'NONE', ( #4597, #6236, #9716, #14210 ) ) ;
#5137 = LINE ( 'NONE', #3175, #10119 ) ;
#5138 = EDGE_CURVE ( 'NONE', #3118, #14145, #6082, .T. ) ;
#5139 = VECTOR ( 'NONE', #4293, 1000.000000000000000 ) ;
#5140 = ORIENTED_EDGE ( 'NONE', *, *, #13248, .F. ) ;
#5141 = UNCERTAINTY_MEASURE_WITH_UNIT (LENGTH_MEASURE( 1.000000000000000082E-05 ), #4992, 'distance_accuracy_value', 'NONE');
#5142 = DIRECTION ( 'NONE',  ( 0.000000000000000000, 0.000000000000000000, -1.000000000000000000 ) ) ;
#5143 = LINE ( 'NONE', #10850, #4360 ) ;
#5144 = LINE ( 'NONE', #11885, #4611 ) ;
#5145 = ORIENTED_EDGE ( 'NONE', *, *, #6298, .T. ) ;
#5146 = CARTESIAN_POINT ( 'NONE',  ( 4.166666666666669627, 3.367876570272813730, -4.118275046351175916 ) ) ;
#5147 = FACE_BOUND ( 'NONE', #8613, .T. ) ;
#5148 = SHAPE_REPRESENTATION_RELATIONSHIP ( 'NONE' , 'NONE' ,  #10940, #5243 ) ;
#5149 = EDGE_LOOP ( 'NONE', ( #13973, #11717, #6274, #14396 ) ) ;
#5150 = ADVANCED_FACE ( 'NONE', ( #6963 ), #6995, .F. ) ;
#5151 = DIRECTION ( 'NONE',  ( -1.000000000000000000, -4.625929269271486900E-16, 0.000000000000000000 ) ) ;
#5152 = ORIENTED_EDGE ( 'NONE', *, *, #7917, .T. ) ;
#5153 = AXIS2_PLACEMENT_3D ( 'NONE', #12494, #12427, #9042 ) ;
#5154 = DIRECTION ( 'NONE',  ( 0.000000000000000000, 0.000000000000000000, -1.000000000000000000 ) ) ;
#5155 = AXIS2_PLACEMENT_3D ( 'NONE', #5009, #14095, #4076 ) ;
#5156 = ORIENTED_EDGE ( 'NONE', *, *, #1606, .F. ) ;
#5157 = FACE_OUTER_BOUND ( 'NONE', #9297, .T. ) ;
#5158 = CARTESIAN_POINT ( 'NONE',  ( 0.000000000000000000, 0.000000000000000000, 0.000000000000000000 ) ) ;
#5159 = EDGE_LOOP ( 'NONE', ( #7101, #5437, #11398 ) ) ;
#5160 = DIRECTION ( 'NONE',  ( -0.9240638205168505426, 0.3822382184081045131, 0.000000000000000000 ) ) ;
#5161 = CARTESIAN_POINT ( 'NONE',  ( 71.80728622811317052, -17.99808865627607801, 25.00000000000000000 ) ) ;
#5162 = ORIENTED_EDGE ( 'NONE', *, *, #1139, .F. ) ;
#5163 = EDGE_LOOP ( 'NONE', ( #3443, #9031, #9692, #6186 ) ) ;
#5164 = AXIS2_PLACEMENT_3D ( 'NONE', #4654, #12604, #7929 ) ;
#5165 = ORIENTED_EDGE ( 'NONE', *, *, #2799, .T. ) ;
#5166 = CARTESIAN_POINT ( 'NONE',  ( 0.000000000000000000, -1.732050807568885631, 0.000000000000000000 ) ) ;
#5167 = CARTESIAN_POINT ( 'NONE',  ( -3.973178806327567258, 47.44387873568886249, 4.532639216498020929 ) ) ;
#5168 = ORIENTED_EDGE ( 'NONE', *, *, #5510, .T. ) ;
#5169 = VECTOR ( 'NONE', #7050, 1000.000000000000114 ) ;
#5170 = CARTESIAN_POINT ( 'NONE',  ( 76.68170757442801744, 39.57655509336063204, -33.00000000000000000 ) ) ;
#5171 = CARTESIAN_POINT ( 'NONE',  ( 105.6817075744280174, 109.5765550933605113, 1.102182119232617753E-14 ) ) ;
#5172 = ADVANCED_FACE ( 'NONE', ( #1859 ), #2969, .F. ) ;
#5173 = CARTESIAN_POINT ( 'NONE',  ( 3.973110223765541793, 0.6902454861566493793, -3.565797985667388481 ) ) ;
#5174 = ORIENTED_EDGE ( 'NONE', *, *, #2234, .T. ) ;
#5175 = EDGE_CURVE ( 'NONE', #4153, #6300, #3182, .T. ) ;
#5176 = CARTESIAN_POINT ( 'NONE',  ( 24.99999999999999289, -4.898587196589414604E-15, 25.00000000000000000 ) ) ;
#5177 = DIRECTION ( 'NONE',  ( 0.000000000000000000, 1.000000000000000000, -0.000000000000000000 ) ) ;
#5178 = VECTOR ( 'NONE', #1759, 1000.000000000000000 ) ;
#5179 = CARTESIAN_POINT ( 'NONE',  ( 1.828356344711646431, 3.563200125723183120, -4.669316179125290331E-15 ) ) ;
#5180 = ORIENTED_EDGE ( 'NONE', *, *, #2187, .T. ) ;
#5181 = DIRECTION ( 'NONE',  ( -1.000000000000000000, 0.000000000000000000, 0.000000000000000000 ) ) ;
#5182 = ORIENTED_EDGE ( 'NONE', *, *, #1555, .F. ) ;
#5183 = VERTEX_POINT ( 'NONE', #5222 ) ;
#5184 = LINE ( 'NONE', #9652, #2331 ) ;
#5185 = CIRCLE ( 'NONE', #4046, 0.2000000000000000944 ) ;
#5186 = VECTOR ( 'NONE', #13070, 1000.000000000000000 ) ;
#5187 = CARTESIAN_POINT ( 'NONE',  ( 105.6817075744280174, 69.57655509336051125, 1.592040838891559450E-14 ) ) ;
#5188 = CARTESIAN_POINT ( 'NONE',  ( 0.5330603548786414514, 48.48645934998781115, 7.973110123615591682 ) ) ;
#5189 = CARTESIAN_POINT ( 'NONE',  ( 5.103279350327459163, -2.353751664345928862, -4.076817471046940256 ) ) ;
#5190 = LINE ( 'NONE', #12970, #9623 ) ;
#5191 = APPLICATION_PROTOCOL_DEFINITION ( 'draft international standard', 'automotive_design', 1998, #4388 ) ;
#5192 = CARTESIAN_POINT ( 'NONE',  ( -4.207491450040565795, 2.029819825146467416, -3.371670828759588456 ) ) ;
#5193 = DIRECTION ( 'NONE',  ( -1.000000000000000000, 0.000000000000000000, 0.000000000000000000 ) ) ;
#5194 = ORIENTED_EDGE ( 'NONE', *, *, #9461, .T. ) ;
#5195 = VECTOR ( 'NONE', #11598, 1000.000000000000000 ) ;
#5196 = CIRCLE ( 'NONE', #14089, 2.500000000000002220 ) ;
#5197 = DIRECTION ( 'NONE',  ( -0.000000000000000000, -0.000000000000000000, 1.000000000000000000 ) ) ;
#5198 = ORIENTED_EDGE ( 'NONE', *, *, #9882, .T. ) ;
#5199 = VERTEX_POINT ( 'NONE', #10786 ) ;
#5200 = VERTEX_POINT ( 'NONE', #5070 ) ;
#5201 = DIRECTION ( 'NONE',  ( -1.000000000000000000, 0.000000000000000000, 0.000000000000000000 ) ) ;
#5202 = CARTESIAN_POINT ( 'NONE',  ( -4.101948962585907132, -2.368261337751098594, -3.381124513963619016 ) ) ;
#5203 = COLOUR_RGB ( '', 0.66274510, 0.83137255, 0.94901961) ;
#5204 = VECTOR ( 'NONE', #8806, 1000.000000000000000 ) ;
#5205 =( NAMED_UNIT ( * ) SI_UNIT ( $, .STERADIAN. ) SOLID_ANGLE_UNIT ( ) );
#5206 = EDGE_CURVE ( 'NONE', #4122, #10954, #884, .T. ) ;
#5207 = EDGE_CURVE ( 'NONE', #12380, #11468, #1177, .T. ) ;
#5208 = ORIENTED_EDGE ( 'NONE', *, *, #4181, .T. ) ;
#5209 = CARTESIAN_POINT ( 'NONE',  ( 1.598077599630167711, -4.850852159564259303, -4.271474537231044089 ) ) ;
#5210 = DIRECTION ( 'NONE',  ( -1.000000000000000000, -0.000000000000000000, -0.000000000000000000 ) ) ;
#5211 = ORIENTED_EDGE ( 'NONE', *, *, #6206, .F. ) ;
#5212 = DIRECTION ( 'NONE',  ( -1.000000000000000000, 0.000000000000000000, 0.000000000000000000 ) ) ;
#5213 = ORIENTED_EDGE ( 'NONE', *, *, #4236, .T. ) ;
#5214 = AXIS2_PLACEMENT_3D ( 'NONE', #12240, #4500, #13267 ) ;
#5215 = VERTEX_POINT ( 'NONE', #14020 ) ;
#5216 = EDGE_CURVE ( 'NONE', #10014, #11757, #767, .T. ) ;
#5217 = CARTESIAN_POINT ( 'NONE',  ( 62.10586122665984732, -20.42344490663941414, 25.00000000000000000 ) ) ;
#5218 = FACE_OUTER_BOUND ( 'NONE', #2388, .T. ) ;
#5219 = CARTESIAN_POINT ( 'NONE',  ( 108.6817075744280743, 59.57655509336061073, 25.00000000000000000 ) ) ;
#5220 = VERTEX_POINT ( 'NONE', #10641 ) ;
#5221 = LINE ( 'NONE', #9467, #3996 ) ;
#5222 = CARTESIAN_POINT ( 'NONE',  ( 24.99999999999999289, -4.898587196589414604E-15, 25.00000000000000000 ) ) ;
#5223 = SHAPE_REPRESENTATION_RELATIONSHIP ( 'NONE' , 'NONE' ,  #8802, #10106 ) ;
#5224 = EDGE_CURVE ( 'NONE', #974, #11904, #628, .T. ) ;
#5225 = ORIENTED_EDGE ( 'NONE', *, *, #7390, .F. ) ;
#5226 = DIRECTION ( 'NONE',  ( 0.000000000000000000, 0.000000000000000000, -1.000000000000000000 ) ) ;
#5227 = AXIS2_PLACEMENT_3D ( 'NONE', #5158, #832, #14030 ) ;
#5228 = ORIENTED_EDGE ( 'NONE', *, *, #12022, .F. ) ;
#5229 = CARTESIAN_POINT ( 'NONE',  ( 6.123233995736776143E-16, 189.5765550933606107, -42.00000000000003553 ) ) ;
#5230 = EDGE_LOOP ( 'NONE', ( #2182, #1447, #10425, #8154, #10660, #3810, #9125, #13761 ) ) ;
#5231 = CARTESIAN_POINT ( 'NONE',  ( 22.00000000000000355, 30.00000000000000711, 25.00000000000000000 ) ) ;
#5232 = VECTOR ( 'NONE', #795, 1000.000000000000000 ) ;
#5233 = ORIENTED_EDGE ( 'NONE', *, *, #11313, .T. ) ;
#5234 = CARTESIAN_POINT ( 'NONE',  ( 1.747541505913290605, -3.837784562140271305, -3.203702292528895157 ) ) ;
#5235 = DIRECTION ( 'NONE',  ( 0.000000000000000000, 0.000000000000000000, 1.000000000000000000 ) ) ;
#5236 = PRODUCT_DEFINITION_FORMATION_WITH_SPECIFIED_SOURCE ( 'ANY', '', #11275, .NOT_KNOWN. ) ;
#5237 = EDGE_CURVE ( 'NONE', #6553, #11217, #11752, .T. ) ;
#5238 = ORIENTED_EDGE ( 'NONE', *, *, #1844, .T. ) ;
#5239 = CYLINDRICAL_SURFACE ( 'NONE', #13893, 10.00000000000000355 ) ;
#5240 = CARTESIAN_POINT ( 'NONE',  ( -3.176101805495866515, 47.84421704054533819, 1.554735638783587337 ) ) ;
#5241 = EDGE_LOOP ( 'NONE', ( #12269, #12765, #9527, #10378 ) ) ;
#5242 = CARTESIAN_POINT ( 'NONE',  ( 5.056385618527004411, -2.321455725013320315, 4.020879263244736990 ) ) ;
#5243 = ADVANCED_BREP_SHAPE_REPRESENTATION ( '', ( #11564, #11025 ), #7056 ) ;
#5244 = AXIS2_PLACEMENT_3D ( 'NONE', #4007, #8377, #9333 ) ;
#5245 = CARTESIAN_POINT ( 'NONE',  ( 4.988724804725785944, -4.618802153517009401, 0.000000000000000000 ) ) ;
#5246 = PLANE ( 'NONE',  #3494 ) ;
#5247 = FACE_OUTER_BOUND ( 'NONE', #12911, .T. ) ;
#5248 = EDGE_CURVE ( 'NONE', #1545, #950, #10713, .T. ) ;
#5249 = VERTEX_POINT ( 'NONE', #11814 ) ;
#5250 = DIRECTION ( 'NONE',  ( 0.000000000000000000, 0.000000000000000000, -1.000000000000000000 ) ) ;
#5251 = DIRECTION ( 'NONE',  ( 0.000000000000000000, 0.000000000000000000, -1.000000000000000000 ) ) ;
#5252 = DIRECTION ( 'NONE',  ( 0.000000000000000000, 0.000000000000000000, 1.000000000000000000 ) ) ;
#5253 = VECTOR ( 'NONE', #13119, 1000.000000000000000 ) ;
#5254 = ORIENTED_EDGE ( 'NONE', *, *, #241, .F. ) ;
#5255 = EDGE_CURVE ( 'NONE', #1219, #12216, #7547, .T. ) ;
#5256 = ADVANCED_FACE ( 'NONE', ( #2900 ), #2004, .T. ) ;
#5257 = ORIENTED_EDGE ( 'NONE', *, *, #10196, .F. ) ;
#5258 = LINE ( 'NONE', #4391, #13431 ) ;
#5259 = EDGE_LOOP ( 'NONE', ( #9666, #6496, #10416, #10841 ) ) ;
#5260 = VERTEX_POINT ( 'NONE', #9822 ) ;
#5261 = CARTESIAN_POINT ( 'NONE',  ( 0.000000000000000000, 25.49999999999996803, 0.000000000000000000 ) ) ;
#5262 = LINE ( 'NONE', #4327, #3508 ) ;
#5263 = DIRECTION ( 'NONE',  ( -1.000000000000000000, -3.286707217423839940E-17, -2.273843122241288053E-18 ) ) ;
#5264 = DIRECTION ( 'NONE',  ( -1.000000000000000000, 0.000000000000000000, 0.000000000000000000 ) ) ;
#5265 = SPHERICAL_SURFACE ( 'NONE', #962, 5.315148208181398104 ) ;
#5266 = PRODUCT_CONTEXT ( 'NONE', #3827, 'mechanical' ) ;
#5267 = CARTESIAN_POINT ( 'NONE',  ( -4.198928548860770604, 0.8158838809860085028, -3.226471437616899252 ) ) ;
#5268 = CARTESIAN_POINT ( 'NONE',  ( 6.250000000000033751, 6.938893903907228378E-15, -1.387778780781445676E-14 ) ) ;
#5269 = VERTEX_POINT ( 'NONE', #9613 ) ;
#5270 = CARTESIAN_POINT ( 'NONE',  ( 22.00000000000000355, 50.00000000000000000, -25.00000000000000000 ) ) ;
#5271 = ORIENTED_EDGE ( 'NONE', *, *, #10702, .T. ) ;
#5272 = ADVANCED_FACE ( 'NONE', ( #694, #5147, #14096, #4077, #6518, #7691, #4359 ), #13276, .T. ) ;
#5273 = EDGE_CURVE ( 'NONE', #2779, #11468, #3253, .T. ) ;
#5274 = CARTESIAN_POINT ( 'NONE',  ( 5.599999999999994316, 7.263589608730915515E-16, 2.499999999999999556 ) ) ;
#5275 = ORIENTED_EDGE ( 'NONE', *, *, #8646, .T. ) ;
#5276 = DIRECTION ( 'NONE',  ( -1.000000000000000000, 0.000000000000000000, 0.000000000000000000 ) ) ;
#5277 = DIRECTION ( 'NONE',  ( 1.000000000000000000, 0.000000000000000000, 0.000000000000000000 ) ) ;
#5278 = ADVANCED_FACE ( 'NONE', ( #966 ), #6761, .T. ) ;
#5279 = VERTEX_POINT ( 'NONE', #9126 ) ;
#5280 = VERTEX_POINT ( 'NONE', #10605 ) ;
#5281 = DIRECTION ( 'NONE',  ( -1.000000000000000000, 0.000000000000000000, 0.000000000000000000 ) ) ;
#5282 = LINE ( 'NONE', #5352, #5640 ) ;
#5283 = LINE ( 'NONE', #13055, #8719 ) ;
#5284 = EDGE_CURVE ( 'NONE', #5967, #7049, #3594, .T. ) ;
#5285 = EDGE_CURVE ( 'NONE', #12157, #7235, #4890, .T. ) ;
#5286 = LINE ( 'NONE', #2895, #12404 ) ;
#5287 = DIRECTION ( 'NONE',  ( 0.000000000000000000, -0.8660254037844388186, 0.4999999999999996114 ) ) ;
#5288 = FACE_OUTER_BOUND ( 'NONE', #13955, .T. ) ;
#5289 = DIRECTION ( 'NONE',  ( -0.000000000000000000, -1.000000000000000000, -0.000000000000000000 ) ) ;
#5290 = CARTESIAN_POINT ( 'NONE',  ( -6.938893903907228378E-15, 24.50000000000002132, 0.000000000000000000 ) ) ;
#5291 = DIRECTION ( 'NONE',  ( 0.7071067811865490160, 1.177569344012833409E-16, 0.7071067811865460184 ) ) ;
#5292 = EDGE_LOOP ( 'NONE', ( #12843, #7817, #748, #2080 ) ) ;
#5293 = ORIENTED_EDGE ( 'NONE', *, *, #5636, .F. ) ;
#5294 = LINE ( 'NONE', #3120, #12559 ) ;
#5295 = EDGE_CURVE ( 'NONE', #13026, #5508, #3662, .T. ) ;
#5296 = FACE_OUTER_BOUND ( 'NONE', #2409, .T. ) ;
#5297 = VERTEX_POINT ( 'NONE', #11472 ) ;
#5298 = DIRECTION ( 'NONE',  ( -0.2425356250363330801, 0.9701425001453319874, 0.000000000000000000 ) ) ;
#5299 = CARTESIAN_POINT ( 'NONE',  ( 20.00000000000000000, 27.00000000000000355, 25.00000000000000000 ) ) ;
#5300 = EDGE_CURVE ( 'NONE', #1210, #992, #12382, .T. ) ;
#5301 = ORIENTED_EDGE ( 'NONE', *, *, #14246, .F. ) ;
#5302 = ORIENTED_EDGE ( 'NONE', *, *, #1174, .F. ) ;
#5303 = DIRECTION ( 'NONE',  ( -0.9701425001453325425, -0.2425356250363304988, 0.000000000000000000 ) ) ;
#5304 = CARTESIAN_POINT ( 'NONE',  ( -3.868826622783372304, 47.50255440539073959, 2.950282236837605154 ) ) ;
#5305 = APPLICATION_CONTEXT ( 'automotive_design' ) ;
#5306 = ORIENTED_EDGE ( 'NONE', *, *, #4727, .T. ) ;
#5307 = AXIS2_PLACEMENT_3D ( 'NONE', #900, #8870, #12177 ) ;
#5308 = DIRECTION ( 'NONE',  ( 0.000000000000000000, 0.000000000000000000, 1.000000000000000000 ) ) ;
#5309 = CARTESIAN_POINT ( 'NONE',  ( -3.999999999999995559, 0.1981133338132423372, 1.817203309215693801E-15 ) ) ;
#5310 = CIRCLE ( 'NONE', #2044, 6.438111078829122036 ) ;
#5311 = DIRECTION ( 'NONE',  ( -0.000000000000000000, 1.000000000000000000, -0.000000000000000000 ) ) ;
#5312 = DIRECTION ( 'NONE',  ( 0.000000000000000000, 0.000000000000000000, -1.000000000000000000 ) ) ;
#5313 = ORIENTED_EDGE ( 'NONE', *, *, #11467, .F. ) ;
#5314 = PRESENTATION_STYLE_ASSIGNMENT (( #5589 ) ) ;
#5315 = CARTESIAN_POINT ( 'NONE',  ( 0.000000000000000000, 0.000000000000000000, -25.00000000000000000 ) ) ;
#5316 = ADVANCED_FACE ( 'NONE', ( #12569, #363, #7143 ), #13837, .F. ) ;
#5317 = CARTESIAN_POINT ( 'NONE',  ( 0.6448876103708376384, 4.246476118072356698, -0.2256878752776751151 ) ) ;
#5318 = AXIS2_PLACEMENT_3D ( 'NONE', #12935, #6249, #706 ) ;
#5319 = B_SPLINE_CURVE_WITH_KNOTS ( 'NONE', 3,
 ( #12235, #2276, #9, #1175, #3314, #2215 ),
 .UNSPECIFIED., .F., .F.,
 ( 4, 2, 4 ),
 ( -3.640115492415446757E-06, 0.0002066546034006449238, 0.0004169493222937052960 ),
 .UNSPECIFIED. ) ;
#5320 = ORIENTED_EDGE ( 'NONE', *, *, #2701, .F. ) ;
#5321 = CARTESIAN_POINT ( 'NONE',  ( 2.930059260563453005, 4.081832189068404837, -8.080694316806025235E-15 ) ) ;
#5322 = ORIENTED_EDGE ( 'NONE', *, *, #13571, .T. ) ;
#5323 = CARTESIAN_POINT ( 'NONE',  ( 76.68170757442796059, 3.003422806631532356E-13, 33.00000000000000000 ) ) ;
#5324 = CARTESIAN_POINT ( 'NONE',  ( 78.52142056027061301, -86.08568224108226730, -28.00000000000000000 ) ) ;
#5325 = AXIS2_PLACEMENT_3D ( 'NONE', #4777, #9229, #13712 ) ;
#5326 = CYLINDRICAL_SURFACE ( 'NONE', #6984, 9.999999999999996447 ) ;
#5327 = CARTESIAN_POINT ( 'NONE',  ( 1.560000000000005826, -0.8660254037844428154, -1.500000000000001332 ) ) ;
#5328 = VECTOR ( 'NONE', #10815, 1000.000000000000000 ) ;
#5329 = CARTESIAN_POINT ( 'NONE',  ( 0.000000000000000000, 4.618802153517016507, -0.5000000000000004441 ) ) ;
#5330 = SHAPE_DEFINITION_REPRESENTATION ( #5759, #4961 ) ;
#5331 = CARTESIAN_POINT ( 'NONE',  ( 3.999999999999999112, -1.700153365594969879, -3.020323189000999164 ) ) ;
#5332 = EDGE_CURVE ( 'NONE', #11217, #11202, #8031, .T. ) ;
#5333 = DIRECTION ( 'NONE',  ( 0.000000000000000000, 1.000000000000000000, 0.000000000000000000 ) ) ;
#5334 = ORIENTED_EDGE ( 'NONE', *, *, #13563, .F. ) ;
#5335 = CARTESIAN_POINT ( 'NONE',  ( 4.175075985190068728, -2.060370777630105010, 3.568666869285572307 ) ) ;
#5336 = ORIENTED_EDGE ( 'NONE', *, *, #3581, .T. ) ;
#5337 = VECTOR ( 'NONE', #8683, 1000.000000000000000 ) ;
#5338 = VECTOR ( 'NONE', #4670, 1000.000000000000000 ) ;
#5339 = DIRECTION ( 'NONE',  ( 0.000000000000000000, 1.000000000000000000, 0.000000000000000000 ) ) ;
#5340 = ORIENTED_EDGE ( 'NONE', *, *, #5062, .F. ) ;
#5341 = DIRECTION ( 'NONE',  ( 0.000000000000000000, 0.000000000000000000, 1.000000000000000000 ) ) ;
#5342 = CARTESIAN_POINT ( 'NONE',  ( -6.209175019847646269E-15, 2.859595677584334528, -2.047034997319569616 ) ) ;
#5343 = SHAPE_REPRESENTATION ( 'Hardened Serrated Safety Wedge', ( #11025 ), #6359 ) ;
#5344 = DIRECTION ( 'NONE',  ( 0.000000000000000000, 0.000000000000000000, 1.000000000000000000 ) ) ;
#5345 = LINE ( 'NONE', #2211, #10438 ) ;
#5346 = FILL_AREA_STYLE ('',( #7598 ) ) ;
#5347 = ADVANCED_FACE ( 'NONE', ( #3731, #12505, #7002, #3811, #12639 ), #5900, .T. ) ;
#5348 = VECTOR ( 'NONE', #13452, 1000.000000000000000 ) ;
#5349 = EDGE_LOOP ( 'NONE', ( #11109, #9631, #13994, #3194 ) ) ;
#5350 = EDGE_CURVE ( 'NONE', #1315, #269, #10758, .T. ) ;
#5351 = FACE_OUTER_BOUND ( 'NONE', #12690, .T. ) ;
#5352 = CARTESIAN_POINT ( 'NONE',  ( 62.10586122665984732, -20.42344490663941414, 23.00000000000000000 ) ) ;
#5353 = DIRECTION ( 'NONE',  ( -0.000000000000000000, 1.000000000000000000, 0.000000000000000000 ) ) ;
#5354 = CARTESIAN_POINT ( 'NONE',  ( -1.287221018261888839, -3.875624752116721528, -3.130620751971867843 ) ) ;
#5355 = VECTOR ( 'NONE', #13607, 1000.000000000000000 ) ;
#5356 = DIRECTION ( 'NONE',  ( 0.000000000000000000, -8.482162385747133845E-47, 1.000000000000000000 ) ) ;
#5357 = PLANE ( 'NONE',  #1813 ) ;
#5358 = CARTESIAN_POINT ( 'NONE',  ( 118.6817075744280316, 69.57655509336046862, 0.000000000000000000 ) ) ;
#5359 = PLANE ( 'NONE',  #10533 ) ;
#5360 = DIRECTION ( 'NONE',  ( 0.000000000000000000, 0.000000000000000000, 1.000000000000000000 ) ) ;
#5361 = CIRCLE ( 'NONE', #1373, 3.299999999999997158 ) ;
#5362 = SURFACE_STYLE_FILL_AREA ( #13145 ) ;
#5363 = CARTESIAN_POINT ( 'NONE',  ( -28.00000000000000355, 35.49999999999997868, 8.000000000000007105 ) ) ;
#5364 = ORIENTED_EDGE ( 'NONE', *, *, #11014, .F. ) ;
#5365 = ORIENTED_EDGE ( 'NONE', *, *, #4614, .F. ) ;
#5366 = FACE_OUTER_BOUND ( 'NONE', #5230, .T. ) ;
#5367 = CARTESIAN_POINT ( 'NONE',  ( 4.175647895129166898, -2.207990717223097921, -3.169390900447838888 ) ) ;
#5368 = CONICAL_SURFACE ( 'NONE', #13564, 5.560781378645576645, 1.221730476396047926 ) ;
#5369 = ORIENTED_EDGE ( 'NONE', *, *, #13087, .F. ) ;
#5370 = FACE_OUTER_BOUND ( 'NONE', #998, .T. ) ;
#5371 = FACE_BOUND ( 'NONE', #6212, .T. ) ;
#5372 = EDGE_LOOP ( 'NONE', ( #11122, #9946, #8180, #13050 ) ) ;
#5373 = VERTEX_POINT ( 'NONE', #591 ) ;
#5374 = DIRECTION ( 'NONE',  ( 0.000000000000000000, 0.000000000000000000, -1.000000000000000000 ) ) ;
#5375 = CARTESIAN_POINT ( 'NONE',  ( -2.015657056808819014, 48.24519377879725113, 0.5351343119442694141 ) ) ;
#5376 = ORIENTED_EDGE ( 'NONE', *, *, #4979, .T. ) ;
#5377 = FACE_OUTER_BOUND ( 'NONE', #7800, .T. ) ;
#5378 = DIRECTION ( 'NONE',  ( 1.000000000000000000, -2.551526159633717598E-19, 1.734723475976770887E-18 ) ) ;
#5379 = DIRECTION ( 'NONE',  ( 0.000000000000000000, 0.000000000000000000, -1.000000000000000000 ) ) ;
#5380 = CARTESIAN_POINT ( 'NONE',  ( -5.211749180171795892, 2.764497899775258283, -4.327903350935040194 ) ) ;
#5381 = ORIENTED_EDGE ( 'NONE', *, *, #12032, .T. ) ;
#5382 = EDGE_CURVE ( 'NONE', #373, #6157, #4818, .T. ) ;
#5383 = EDGE_CURVE ( 'NONE', #12126, #260, #1676, .T. ) ;
#5384 = CYLINDRICAL_SURFACE ( 'NONE', #8128, 2.000000000000001776 ) ;
#5385 = DIRECTION ( 'NONE',  ( -0.000000000000000000, 1.000000000000000000, -0.000000000000000000 ) ) ;
#5386 = CIRCLE ( 'NONE', #21, 0.2000000000000000944 ) ;
#5387 =( GEOMETRIC_REPRESENTATION_CONTEXT ( 3 ) GLOBAL_UNCERTAINTY_ASSIGNED_CONTEXT ( ( #4713 ) ) GLOBAL_UNIT_ASSIGNED_CONTEXT ( ( #5031, #4105, #4168 ) ) REPRESENTATION_CONTEXT ( 'NONE', 'WORKASPACE' ) );
#5388 = AXIS2_PLACEMENT_3D ( 'NONE', #12247, #7839, #12315 ) ;
#5389 = ORIENTED_EDGE ( 'NONE', *, *, #1565, .F. ) ;
#5390 = VERTEX_POINT ( 'NONE', #12722 ) ;
#5391 = CARTESIAN_POINT ( 'NONE',  ( 78.52142056027055617, 29.57655509336062849, -28.00000000000000000 ) ) ;
#5392 = EDGE_CURVE ( 'NONE', #13612, #9296, #4967, .T. ) ;
#5393 = ADVANCED_FACE ( 'NONE', ( #294 ), #11694, .T. ) ;
#5394 = VECTOR ( 'NONE', #11265, 1000.000000000000000 ) ;
#5395 = VERTEX_POINT ( 'NONE', #10527 ) ;
#5396 = CARTESIAN_POINT ( 'NONE',  ( 3.961545574369877531, 1.423222908132143250, -3.499999999999992450 ) ) ;
#5397 = DIRECTION ( 'NONE',  ( -2.243905293393255080E-15, 8.975621173573017164E-15, 1.000000000000000000 ) ) ;
#5398 = ORIENTED_EDGE ( 'NONE', *, *, #2893, .F. ) ;
#5399 = DIRECTION ( 'NONE',  ( 1.000000000000000000, 0.000000000000000000, 0.000000000000000000 ) ) ;
#5400 = CIRCLE ( 'NONE', #4940, 6.726859516510133474 ) ;
#5401 = DIRECTION ( 'NONE',  ( 0.5000000000000009992, -0.8660254037844380415, 0.000000000000000000 ) ) ;
#5402 =( GEOMETRIC_REPRESENTATION_CONTEXT ( 3 ) GLOBAL_UNCERTAINTY_ASSIGNED_CONTEXT ( ( #2665 ) ) GLOBAL_UNIT_ASSIGNED_CONTEXT ( ( #2975, #6174, #10648 ) ) REPRESENTATION_CONTEXT ( 'NONE', 'WORKASPACE' ) );
#5403 = PLANE ( 'NONE',  #4028 ) ;
#5404 = CARTESIAN_POINT ( 'NONE',  ( 3.999999999999999112, -2.471526491860384311, -3.386887032901821470 ) ) ;
#5405 = AXIS2_PLACEMENT_3D ( 'NONE', #8193, #11490, #12584 ) ;
#5406 = CARTESIAN_POINT ( 'NONE',  ( 4.175326769692829565, 2.060699556488938100, -3.569236330973477589 ) ) ;
#5407 = ORIENTED_EDGE ( 'NONE', *, *, #4684, .T. ) ;
#5408 = DIRECTION ( 'NONE',  ( 0.000000000000000000, -0.000000000000000000, 1.000000000000000000 ) ) ;
#5409 = ORIENTED_EDGE ( 'NONE', *, *, #350, .T. ) ;
#5410 = VECTOR ( 'NONE', #14065, 1000.000000000000000 ) ;
#5411 = AXIS2_PLACEMENT_3D ( 'NONE', #9660, #6283, #7383 ) ;
#5412 = CARTESIAN_POINT ( 'NONE',  ( 20.00000000000000355, 50.00000000000000000, -25.00000000000000000 ) ) ;
#5413 = EDGE_CURVE ( 'NONE', #337, #4861, #509, .T. ) ;
#5414 = DIRECTION ( 'NONE',  ( 1.734723475976770502E-18, -4.440892098500621231E-16, -1.000000000000000000 ) ) ;
#5415 = CARTESIAN_POINT ( 'NONE',  ( 108.6817075744280459, 109.5765550933604828, 0.000000000000000000 ) ) ;
#5416 = DIRECTION ( 'NONE',  ( -0.2425356250363328581, 0.9701425001453318764, 0.000000000000000000 ) ) ;
#5417 = PLANE ( 'NONE',  #1923 ) ;
#5418 = ADVANCED_FACE ( 'NONE', ( #6128 ), #8173, .F. ) ;
#5419 = EDGE_LOOP ( 'NONE', ( #12431, #2655, #7706, #10350, #6054 ) ) ;
#5420 = VECTOR ( 'NONE', #10553, 1000.000000000000114 ) ;
#5421 = CONICAL_SURFACE ( 'NONE', #14314, 4.000000000000000000, 0.8911886515913775009 ) ;
#5422 = FACE_OUTER_BOUND ( 'NONE', #11714, .T. ) ;
#5423 = LINE ( 'NONE', #1106, #9398 ) ;
#5424 = CARTESIAN_POINT ( 'NONE',  ( 79.68170757442804586, 59.57655509336061073, 25.00000000000000000 ) ) ;
#5425 = CARTESIAN_POINT ( 'NONE',  ( 0.000000000000000000, 40.49999999999999289, 8.000000000000007105 ) ) ;
#5426 = STYLED_ITEM ( 'NONE', ( #11213 ), #1042 ) ;
#5427 = EDGE_CURVE ( 'NONE', #7396, #9797, #5041, .T. ) ;
#5428 = AXIS2_PLACEMENT_3D ( 'NONE', #12377, #12, #2351 ) ;
#5429 = ADVANCED_FACE ( 'NONE', ( #8481 ), #7374, .F. ) ;
#5430 = VECTOR ( 'NONE', #4987, 1000.000000000000000 ) ;
#5431 = CARTESIAN_POINT ( 'NONE',  ( 4.000000000000003553, -1.539600717839009203, -3.000726591567076440 ) ) ;
#5432 = CARTESIAN_POINT ( 'NONE',  ( 1.560000000000005826, 1.299038105676664223, 0.7500000000000006661 ) ) ;
#5433 = CARTESIAN_POINT ( 'NONE',  ( 6.250000000000033751, 4.928740591811433280E-15, -6.250000000000021316 ) ) ;
#5434 = DIRECTION ( 'NONE',  ( -1.000000000000000000, 0.000000000000000000, 0.000000000000000000 ) ) ;
#5435 = DIRECTION ( 'NONE',  ( 0.000000000000000000, -1.000000000000000000, 0.000000000000000000 ) ) ;
#5436 = DIRECTION ( 'NONE',  ( 0.000000000000000000, 0.000000000000000000, 1.000000000000000000 ) ) ;
#5437 = ORIENTED_EDGE ( 'NONE', *, *, #5285, .T. ) ;
#5438 = ORIENTED_EDGE ( 'NONE', *, *, #674, .T. ) ;
#5439 = LINE ( 'NONE', #4364, #2049 ) ;
#5440 = VECTOR ( 'NONE', #7656, 1000.000000000000000 ) ;
#5441 = DIRECTION ( 'NONE',  ( 1.000000000000000000, 0.000000000000000000, 0.000000000000000000 ) ) ;
#5442 = ORIENTED_EDGE ( 'NONE', *, *, #11403, .F. ) ;
#5443 = DIRECTION ( 'NONE',  ( 0.000000000000000000, 0.000000000000000000, -1.000000000000000000 ) ) ;
#5444 = CARTESIAN_POINT ( 'NONE',  ( 51.83050351964435976, 32.98574998546678927, 25.00000000000000000 ) ) ;
#5445 = ORIENTED_EDGE ( 'NONE', *, *, #12914, .F. ) ;
#5446 = ORIENTED_EDGE ( 'NONE', *, *, #1453, .F. ) ;
#5447 = CARTESIAN_POINT ( 'NONE',  ( -1.391697335622804621, -4.043246145443390560, -3.203898532754352768 ) ) ;
#5448 = CARTESIAN_POINT ( 'NONE',  ( 20.00000000000000000, 27.00000000000000355, -25.00000000000000000 ) ) ;
#5449 = FACE_OUTER_BOUND ( 'NONE', #8596, .T. ) ;
#5450 = VECTOR ( 'NONE', #11131, 1000.000000000000000 ) ;
#5451 = CARTESIAN_POINT ( 'NONE',  ( 22.00000000000000711, 20.00000000000000355, 25.00000000000000000 ) ) ;
#5452 = PRODUCT_DEFINITION_SHAPE ( 'NONE', 'NONE',  #14490 ) ;
#5453 = LINE ( 'NONE', #10873, #14206 ) ;
#5454 = CARTESIAN_POINT ( 'NONE',  ( -3.514986608503188670, 4.017641317387355748, -4.357689166958564009 ) ) ;
#5455 = VERTEX_POINT ( 'NONE', #1755 ) ;
#5456 = SURFACE_SIDE_STYLE ('',( #3141 ) ) ;
#5457 = AXIS2_PLACEMENT_3D ( 'NONE', #6271, #7371, #5181 ) ;
#5458 = CARTESIAN_POINT ( 'NONE',  ( -3.567687560464433361, 3.713697318477639620, -0.1121614189353362934 ) ) ;
#5459 = CARTESIAN_POINT ( 'NONE',  ( 0.000000000000000000, 0.000000000000000000, 0.000000000000000000 ) ) ;
#5460 = AXIS2_PLACEMENT_3D ( 'NONE', #3962, #10314, #11704 ) ;
#5461 = ORIENTED_EDGE ( 'NONE', *, *, #8753, .T. ) ;
#5462 = VERTEX_POINT ( 'NONE', #3955 ) ;
#5463 = B_SPLINE_CURVE_WITH_KNOTS ( 'NONE', 3,
 ( #5989, #2357, #10399, #13644 ),
 .UNSPECIFIED., .F., .F.,
 ( 4, 4 ),
 ( 0.000000000000000000, 0.002080789711329283660 ),
 .UNSPECIFIED. ) ;
#5464 = VERTEX_POINT ( 'NONE', #6276 ) ;
#5465 = AXIS2_PLACEMENT_3D ( 'NONE', #6832, #12468, #11298 ) ;
#5466 = EDGE_CURVE ( 'NONE', #13885, #6928, #6, .T. ) ;
#5467 = DIRECTION ( 'NONE',  ( 1.000000000000000000, 1.665334536937734071E-16, 0.000000000000000000 ) ) ;
#5468 = ORIENTED_EDGE ( 'NONE', *, *, #11730, .T. ) ;
#5469 = CARTESIAN_POINT ( 'NONE',  ( 4.180232103119972287, 2.085387772176683807, -3.570466442734691270 ) ) ;
#5470 = CARTESIAN_POINT ( 'NONE',  ( 31.80000000000005045, 6.938893903907228378E-15, 2.775557561562891351E-14 ) ) ;
#5471 = CARTESIAN_POINT ( 'NONE',  ( 3.667453972563985829E-15, 6.066067634115573703, -4.659491423763650886 ) ) ;
#5472 = FACE_OUTER_BOUND ( 'NONE', #1335, .T. ) ;
#5473 = CARTESIAN_POINT ( 'NONE',  ( 5.236872748402767286, 8.765285303662936917E-14, -4.357689166958464533 ) ) ;
#5474 = FACE_OUTER_BOUND ( 'NONE', #2784, .T. ) ;
#5475 = CARTESIAN_POINT ( 'NONE',  ( 34.92765351673772045, 110.5971499970933536, 25.00000000000000000 ) ) ;
#5476 = VECTOR ( 'NONE', #4479, 999.9999999999998863 ) ;
#5477 = ORIENTED_EDGE ( 'NONE', *, *, #7163, .T. ) ;
#5478 = ADVANCED_FACE ( 'NONE', ( #1824 ), #3150, .F. ) ;
#5479 = CARTESIAN_POINT ( 'NONE',  ( 5.599999999999994316, 2.886579864025407597E-16, 5.200000000000001066 ) ) ;
#5480 = EDGE_LOOP ( 'NONE', ( #8376, #5381, #2658, #12612 ) ) ;
#5481 = EDGE_CURVE ( 'NONE', #11750, #3225, #6479, .T. ) ;
#5482 = VERTEX_POINT ( 'NONE', #9507 ) ;
#5483 = VERTEX_POINT ( 'NONE', #8620 ) ;
#5484 = DIRECTION ( 'NONE',  ( -0.2425356250363328581, 0.9701425001453318764, 0.000000000000000000 ) ) ;
#5485 = FACE_OUTER_BOUND ( 'NONE', #6269, .T. ) ;
#5486 = CARTESIAN_POINT ( 'NONE',  ( 0.000000000000000000, -0.8660254037844428154, -1.500000000000001332 ) ) ;
#5487 = EDGE_LOOP ( 'NONE', ( #13801, #4538, #272, #5553, #2751, #5649, #7641, #428, #12183, #578, #8339, #128 ) ) ;
#5488 = CARTESIAN_POINT ( 'NONE',  ( 5.085139881807305251, 2.270820054029174528, -4.066824291575160899 ) ) ;
#5489 = CARTESIAN_POINT ( 'NONE',  ( 108.6817075744280174, 29.57655509336062849, 33.00000000000002842 ) ) ;
#5490 = DIRECTION ( 'NONE',  ( 1.000000000000000000, 0.000000000000000000, 0.000000000000000000 ) ) ;
#5491 = EDGE_CURVE ( 'NONE', #9142, #8011, #2862, .T. ) ;
#5492 = LINE ( 'NONE', #9961, #4270 ) ;
#5493 = ORIENTED_EDGE ( 'NONE', *, *, #7052, .T. ) ;
#5494 = CARTESIAN_POINT ( 'NONE',  ( 129.3408537872138595, 199.5765550933606107, -69.99999999999998579 ) ) ;
#5495 = EDGE_CURVE ( 'NONE', #29, #687, #7507, .T. ) ;
#5496 = CARTESIAN_POINT ( 'NONE',  ( 22.00000000000000355, 50.00000000000000000, 25.00000000000000000 ) ) ;
#5497 =( REPRESENTATION_RELATIONSHIP ('NONE','NONE', #10295, #4961 ) REPRESENTATION_RELATIONSHIP_WITH_TRANSFORMATION ( #420 )SHAPE_REPRESENTATION_RELATIONSHIP( ) );
#5498 = PLANE ( 'NONE',  #13650 ) ;
#5499 = DIRECTION ( 'NONE',  ( 0.000000000000000000, 0.000000000000000000, 1.000000000000000000 ) ) ;
#5500 = ADVANCED_FACE ( 'NONE', ( #13102 ), #1973, .T. ) ;
#5501 = CARTESIAN_POINT ( 'NONE',  ( -140.0000000000003411, 189.5765550933606107, -132.0000000000000000 ) ) ;
#5502 = CARTESIAN_POINT ( 'NONE',  ( 20.00000000000000000, 37.00000000000000711, -25.00000000000000000 ) ) ;
#5503 = CARTESIAN_POINT ( 'NONE',  ( -3.999999999999996447, 2.309401076758494487, -4.699999999999981526 ) ) ;
#5504 = CARTESIAN_POINT ( 'NONE',  ( 4.050823680195247078, -3.779313952391379683, 0.5899027668435089522 ) ) ;
#5505 = AXIS2_PLACEMENT_3D ( 'NONE', #7465, #10637, #6381 ) ;
#5506 = CARTESIAN_POINT ( 'NONE',  ( -129.3408537872145132, 189.5765550933606107, -9.000000000000007105 ) ) ;
#5507 = ORIENTED_EDGE ( 'NONE', *, *, #5027, .T. ) ;
#5508 = VERTEX_POINT ( 'NONE', #798 ) ;
#5509 = DIRECTION ( 'NONE',  ( -1.000000000000000000, 0.000000000000000000, 0.000000000000000000 ) ) ;
#5510 = EDGE_CURVE ( 'NONE', #1722, #9071, #10956, .T. ) ;
#5511 =( LENGTH_UNIT ( ) NAMED_UNIT ( * ) SI_UNIT ( .MILLI., .METRE. ) );
#5512 = ORIENTED_EDGE ( 'NONE', *, *, #967, .F. ) ;
#5513 = LINE ( 'NONE', #3259, #8334 ) ;
#5514 =( BOUNDED_SURFACE ( )  B_SPLINE_SURFACE ( 3, 2, ( 
 ( #12313, #9900, #4356 ),
 ( #12383, #13350, #2285 ),
 ( #3327, #5637, #7771 ),
 ( #8791, #12244, #2356 ),
 ( #6814, #13273, #5766 ),
 ( #11636, #8045, #13708 ) ),
 .UNSPECIFIED., .F., .F., .F. ) 
 B_SPLINE_SURFACE_WITH_KNOTS ( ( 4, 2, 4 ),
 ( 3, 3 ),
 ( 0.01886032586153030266, 0.02121253401777973419, 0.02356474217402916571 ),
 ( 0.000000000000000000, 1.000000000000000000 ),
 .UNSPECIFIED. ) 
 GEOMETRIC_REPRESENTATION_ITEM ( )  RATIONAL_B_SPLINE_SURFACE ( (
 ( 1.000000000000000000, 0.8047781103519395796, 1.000000000000000000),
 ( 1.000000000000000000, 0.8123785825777626313, 1.000000000000000000),
 ( 1.000000000000000000, 0.8190671539557564662, 1.000000000000000000),
 ( 1.000000000000000000, 0.8192352255065570299, 1.000000000000000000),
 ( 1.000000000000000000, 0.8126129677038341770, 1.000000000000000000),
 ( 1.000000000000000000, 0.8047712537969725632, 1.000000000000000000) ) ) 
 REPRESENTATION_ITEM ( '' )  SURFACE ( )  );
#5515 = CARTESIAN_POINT ( 'NONE',  ( 0.1391502195351393967, 2.687187980154705613, 3.345653888883665772 ) ) ;
#5516 = ORIENTED_EDGE ( 'NONE', *, *, #13533, .T. ) ;
#5517 = VERTEX_POINT ( 'NONE', #9787 ) ;
#5518 = CARTESIAN_POINT ( 'NONE',  ( 71.80728622811317052, -20.42344490663941414, 28.00000000000000000 ) ) ;
#5519 = DIRECTION ( 'NONE',  ( -1.000000000000000000, 0.000000000000000000, 0.000000000000000000 ) ) ;
#5520 = DIRECTION ( 'NONE',  ( 1.000000000000000000, 1.665334536937734071E-16, 0.000000000000000000 ) ) ;
#5521 = CARTESIAN_POINT ( 'NONE',  ( -3.999999999999996447, -2.309401076758511806, -0.5000000000000004441 ) ) ;
#5522 = CARTESIAN_POINT ( 'NONE',  ( 105.6817075744280174, 109.5765550933605113, 3.300000000000008260 ) ) ;
#5523 = DIRECTION ( 'NONE',  ( 0.000000000000000000, 0.000000000000000000, -1.000000000000000000 ) ) ;
#5524 = CARTESIAN_POINT ( 'NONE',  ( 5.103531824934171013, 2.354098498486459246, -4.077418205400141105 ) ) ;
#5525 = ADVANCED_FACE ( 'NONE', ( #7305 ), #14261, .F. ) ;
#5526 = EDGE_CURVE ( 'NONE', #9673, #5260, #4222, .T. ) ;
#5527 = CARTESIAN_POINT ( 'NONE',  ( 3.961551342853779190, 2.319461885623249398, 2.982574167880994498 ) ) ;
#5528 = AXIS2_PLACEMENT_3D ( 'NONE', #12031, #2002, #13351 ) ;
#5529 = ORIENTED_EDGE ( 'NONE', *, *, #8616, .F. ) ;
#5530 = DIRECTION ( 'NONE',  ( -1.000000000000000000, 2.551526159633733968E-19, 1.987661601597216239E-18 ) ) ;
#5531 = VERTEX_POINT ( 'NONE', #4252 ) ;
#5532 = VECTOR ( 'NONE', #5988, 1000.000000000000000 ) ;
#5533 = CARTESIAN_POINT ( 'NONE',  ( -3.822382184081044798, 10.25936179483149324, 8.000000000000007105 ) ) ;
#5534 = DIRECTION ( 'NONE',  ( 0.000000000000000000, 0.000000000000000000, -1.000000000000000000 ) ) ;
#5535 = DIRECTION ( 'NONE',  ( -1.000000000000000000, 0.000000000000000000, 0.000000000000000000 ) ) ;
#5536 = DIRECTION ( 'NONE',  ( 0.000000000000000000, 8.482162385747133845E-47, -1.000000000000000000 ) ) ;
#5537 = CARTESIAN_POINT ( 'NONE',  ( 3.972709601346610331, 3.429395227388317924, 1.191688283765310219 ) ) ;
#5538 = LINE ( 'NONE', #10010, #6079 ) ;
#5539 = CARTESIAN_POINT ( 'NONE',  ( 4.165266963751699691, 2.049631966911994230, -3.550066703508909960 ) ) ;
#5540 = CIRCLE ( 'NONE', #6935, 8.000000000000000000 ) ;
#5541 = EDGE_CURVE ( 'NONE', #9296, #7346, #5184, .T. ) ;
#5542 = EDGE_CURVE ( 'NONE', #535, #3862, #8690, .T. ) ;
#5543 = DIRECTION ( 'NONE',  ( 1.000000000000000000, 0.000000000000000000, 0.000000000000000000 ) ) ;
#5544 = ORIENTED_EDGE ( 'NONE', *, *, #1198, .F. ) ;
#5545 = ADVANCED_FACE ( 'NONE', ( #6208 ), #5368, .T. ) ;
#5546 = CARTESIAN_POINT ( 'NONE',  ( 37.27836601746437850, 91.19429999418670718, -25.00000000000000000 ) ) ;
#5547 = VECTOR ( 'NONE', #6391, 1000.000000000000000 ) ;
#5548 = ORIENTED_EDGE ( 'NONE', *, *, #13094, .T. ) ;
#5549 = AXIS2_PLACEMENT_3D ( 'NONE', #5315, #1748, #718 ) ;
#5550 = CARTESIAN_POINT ( 'NONE',  ( 54.35294117647056567, -1.411764705882362358, -23.00000000000000000 ) ) ;
#5551 = CARTESIAN_POINT ( 'NONE',  ( 5.000000000000001776, 2.886751345948152192, -0.5999999999999894307 ) ) ;
#5552 = EDGE_CURVE ( 'NONE', #7346, #9008, #5108, .T. ) ;
#5553 = ORIENTED_EDGE ( 'NONE', *, *, #11256, .F. ) ;
#5554 = CARTESIAN_POINT ( 'NONE',  ( 4.844561581013301144, 3.066321291060833065, -2.688975731552607940 ) ) ;
#5555 = CARTESIAN_POINT ( 'NONE',  ( 0.000000000000000000, 0.000000000000000000, 2.400000000000013234 ) ) ;
#5556 = DIRECTION ( 'NONE',  ( -1.000000000000000000, 0.000000000000000000, 0.000000000000000000 ) ) ;
#5557 = ORIENTED_EDGE ( 'NONE', *, *, #13465, .T. ) ;
#5558 = ADVANCED_FACE ( 'NONE', ( #14131 ), #4115, .F. ) ;
#5559 = EDGE_CURVE ( 'NONE', #11907, #4680, #10150, .T. ) ;
#5560 = LINE ( 'NONE', #2140, #423 ) ;
#5561 = AXIS2_PLACEMENT_3D ( 'NONE', #5734, #6777, #12493 ) ;
#5562 = DIRECTION ( 'NONE',  ( -0.000000000000000000, -0.5000000000000011102, -0.8660254037844379305 ) ) ;
#5563 = VECTOR ( 'NONE', #10806, 1000.000000000000000 ) ;
#5564 = CARTESIAN_POINT ( 'NONE',  ( 31.80000000000005045, 6.938893903907228378E-15, 2.775557561562891351E-14 ) ) ;
#5565 = ADVANCED_BREP_SHAPE_REPRESENTATION ( '', ( #11938, #11025 ), #4496 ) ;
#5566 = CYLINDRICAL_SURFACE ( 'NONE', #2355, 2.500000000000002220 ) ;
#5567 = DIRECTION ( 'NONE',  ( -1.000000000000000000, 0.000000000000000000, 0.000000000000000000 ) ) ;
#5568 = DIRECTION ( 'NONE',  ( 0.000000000000000000, 0.000000000000000000, 1.000000000000000000 ) ) ;
#5569 = EDGE_CURVE ( 'NONE', #10014, #13737, #14408, .T. ) ;
#5570 = EDGE_CURVE ( 'NONE', #3442, #10880, #13527, .T. ) ;
#5571 = FACE_OUTER_BOUND ( 'NONE', #12119, .T. ) ;
#5572 = CARTESIAN_POINT ( 'NONE',  ( 4.844552896834077416, 0.7953914966942765563, 4.000000000000002665 ) ) ;
#5573 = ORIENTED_EDGE ( 'NONE', *, *, #9596, .F. ) ;
#5574 = APPLICATION_CONTEXT ( 'automotive_design' ) ;
#5575 = DIRECTION ( 'NONE',  ( -0.2425356250363328581, 0.9701425001453318764, 0.000000000000000000 ) ) ;
#5576 =( LENGTH_UNIT ( ) NAMED_UNIT ( * ) SI_UNIT ( .MILLI., .METRE. ) );
#5577 = EDGE_LOOP ( 'NONE', ( #1286, #5507, #8075, #7936, #12667, #10442, #1814, #4734, #12975 ) ) ;
#5578 = CARTESIAN_POINT ( 'NONE',  ( 49.47979101891770171, 52.38859998837343568, -25.00000000000000000 ) ) ;
#5579 = VERTEX_POINT ( 'NONE', #9035 ) ;
#5580 = VECTOR ( 'NONE', #2788, 1000.000000000000000 ) ;
#5581 = CARTESIAN_POINT ( 'NONE',  ( -0.8144415599836899444, 5.303284638000468121, -0.2680587191991168350 ) ) ;
#5582 = LINE ( 'NONE', #3483, #1211 ) ;
#5583 = ADVANCED_FACE ( 'NONE', ( #12348 ), #2354, .F. ) ;
#5584 = CARTESIAN_POINT ( 'NONE',  ( 4.180231891692621993, -2.049421325483208989, -3.591231015387289727 ) ) ;
#5585 = LINE ( 'NONE', #10058, #2530 ) ;
#5586 = CARTESIAN_POINT ( 'NONE',  ( 2.888823775385669489E-13, -4.796980096169635388, -3.421999068284433676 ) ) ;
#5587 = LINE ( 'NONE', #9167, #8117 ) ;
#5588 = ORIENTED_EDGE ( 'NONE', *, *, #773, .T. ) ;
#5589 = SURFACE_STYLE_USAGE ( .BOTH. , #5456 ) ;
#5590 = EDGE_LOOP ( 'NONE', ( #2722, #5742, #12452, #8480 ) ) ;
#5592 = ADVANCED_FACE ( 'NONE', ( #7728 ), #5598, .T. ) ;
#5591 = DIRECTION ( 'NONE',  ( 0.000000000000000000, 5.551115123125782702E-17, 1.000000000000000000 ) ) ;
#5593 = VECTOR ( 'NONE', #4558, 1000.000000000000227 ) ;
#5594 = CARTESIAN_POINT ( 'NONE',  ( 108.6817075744280316, -30.42344490663958112, -32.00000000000002842 ) ) ;
#5595 = VERTEX_POINT ( 'NONE', #2189 ) ;
#5596 = ORIENTED_EDGE ( 'NONE', *, *, #3970, .F. ) ;
#5597 = ORIENTED_EDGE ( 'NONE', *, *, #6493, .F. ) ;
#5598 = CONICAL_SURFACE ( 'NONE', #227, 2.055000000000000160, 0.7853981633974428389 ) ;
#5599 = DIRECTION ( 'NONE',  ( -8.619211990076296383E-16, 1.000000000000000000, 0.000000000000000000 ) ) ;
#5600 = EDGE_CURVE ( 'NONE', #11470, #11163, #2321, .T. ) ;
#5601 = ORIENTED_EDGE ( 'NONE', *, *, #10428, .T. ) ;
#5602 = CARTESIAN_POINT ( 'NONE',  ( 3.974167765203679537, 0.7238254970443265268, -3.565825589389254979 ) ) ;
#5603 = ADVANCED_FACE ( 'NONE', ( #11098 ), #8899, .T. ) ;
#5604 = CARTESIAN_POINT ( 'NONE',  ( -5.000000000000000888, -1.947799557644009694, -0.2684016432552358000 ) ) ;
#5605 = DIRECTION ( 'NONE',  ( -1.000000000000000000, -3.286707217423839940E-17, -2.273843122241288053E-18 ) ) ;
#5606 = DIRECTION ( 'NONE',  ( 0.000000000000000000, 0.000000000000000000, 1.000000000000000000 ) ) ;
#5607 = DIRECTION ( 'NONE',  ( 0.000000000000000000, 0.000000000000000000, 1.000000000000000000 ) ) ;
#5608 = CONTEXT_DEPENDENT_SHAPE_REPRESENTATION ( #4499, #7172 ) ;
#5609 = CARTESIAN_POINT ( 'NONE',  ( 4.211140560182194292, -2.431303136016548017, -3.445885042887453231 ) ) ;
#5610 = LINE ( 'NONE', #1013, #12433 ) ;
#5611 = AXIS2_PLACEMENT_3D ( 'NONE', #2169, #11087, #11222 ) ;
#5612 = CARTESIAN_POINT ( 'NONE',  ( 2.426025403784448642, 0.000000000000000000, 2.168404344971008868E-16 ) ) ;
#5613 = ORIENTED_EDGE ( 'NONE', *, *, #13008, .F. ) ;
#5614 = VERTEX_POINT ( 'NONE', #14337 ) ;
#5615 = DIRECTION ( 'NONE',  ( 0.000000000000000000, 0.000000000000000000, -1.000000000000000000 ) ) ;
#5616 = ORIENTED_EDGE ( 'NONE', *, *, #11024, .F. ) ;
#5617 = VECTOR ( 'NONE', #1230, 1000.000000000000227 ) ;
#5618 = VERTEX_POINT ( 'NONE', #11170 ) ;
#5619 = DIRECTION ( 'NONE',  ( 0.000000000000000000, 0.000000000000000000, -1.000000000000000000 ) ) ;
#5620 = VECTOR ( 'NONE', #3491, 1000.000000000000000 ) ;
#5621 = CARTESIAN_POINT ( 'NONE',  ( 31.80000000000005045, 8.024914066595556114E-15, 2.445500000000030649 ) ) ;
#5622 = FILL_AREA_STYLE ('',( #10095 ) ) ;
#5623 = AXIS2_PLACEMENT_3D ( 'NONE', #4139, #5142, #2067 ) ;
#5624 = DIRECTION ( 'NONE',  ( -1.000000000000000000, -1.723842398015259277E-15, 0.000000000000000000 ) ) ;
#5625 = EDGE_LOOP ( 'NONE', ( #10950, #3394, #286, #13456 ) ) ;
#5626 = DIRECTION ( 'NONE',  ( 1.734723475976770502E-18, -4.440892098500621231E-16, -1.000000000000000000 ) ) ;
#5627 = CYLINDRICAL_SURFACE ( 'NONE', #2615, 5.000000000000018652 ) ;
#5628 = DIRECTION ( 'NONE',  ( -4.664070103548417302E-16, 0.9242245927363028635, 0.3818493186865932754 ) ) ;
#5629 = CARTESIAN_POINT ( 'NONE',  ( 28.00000000000000355, 29.99999999999999645, 25.00000000000000000 ) ) ;
#5630 = ORIENTED_EDGE ( 'NONE', *, *, #2575, .T. ) ;
#5631 = CARTESIAN_POINT ( 'NONE',  ( -2.749999999999997780, 25.49999999999996803, 8.000000000000007105 ) ) ;
#5632 = CIRCLE ( 'NONE', #7970, 2.100000000000000977 ) ;
#5633 = AXIS2_PLACEMENT_3D ( 'NONE', #2263, #13467, #8980 ) ;
#5634 = LINE ( 'NONE', #7832, #7769 ) ;
#5635 = CARTESIAN_POINT ( 'NONE',  ( 22.28098402457126426, 141.4229888148238103, 1.219362754841566419E-12 ) ) ;
#5636 = EDGE_CURVE ( 'NONE', #2267, #12223, #4326, .T. ) ;
#5637 = CARTESIAN_POINT ( 'NONE',  ( 4.847001880571981225, -3.878482749467707880, 1.282270821642251368 ) ) ;
#5638 = DIRECTION ( 'NONE',  ( -1.000000000000000000, 0.000000000000000000, 0.000000000000000000 ) ) ;
#5639 = LINE ( 'NONE', #13913, #13321 ) ;
#5640 = VECTOR ( 'NONE', #6226, 1000.000000000000000 ) ;
#5641 = VECTOR ( 'NONE', #12730, 1000.000000000000000 ) ;
#5642 = CARTESIAN_POINT ( 'NONE',  ( 4.847010933397505106, -0.8288363800944087423, 4.000000000000002665 ) ) ;
#5643 = DIRECTION ( 'NONE',  ( 1.000000000000000000, 1.224646799147353454E-16, 0.000000000000000000 ) ) ;
#5644 = ORIENTED_EDGE ( 'NONE', *, *, #662, .F. ) ;
#5645 = EDGE_CURVE ( 'NONE', #4075, #2107, #12130, .T. ) ;
#5646 = DIRECTION ( 'NONE',  ( 0.000000000000000000, 1.000000000000000000, 0.000000000000000000 ) ) ;
#5647 = CIRCLE ( 'NONE', #7759, 3.499999999999999112 ) ;
#5648 = PRODUCT ( 'link rod', 'link rod', '', ( #11929 ) ) ;
#5649 = ORIENTED_EDGE ( 'NONE', *, *, #13995, .T. ) ;
#5650 = EDGE_CURVE ( 'NONE', #4147, #13213, #12277, .T. ) ;
#5651 = CARTESIAN_POINT ( 'NONE',  ( 20.00000000000000000, -5.510910596163090344E-15, -25.00000000000000000 ) ) ;
#5652 = LINE ( 'NONE', #7784, #1687 ) ;
#5653 = FACE_OUTER_BOUND ( 'NONE', #8593, .T. ) ;
#5654 = CARTESIAN_POINT ( 'NONE',  ( 95.04167153547044222, -149.6197612287760705, -28.00000000000000000 ) ) ;
#5655 = DIRECTION ( 'NONE',  ( 1.840274199520074535E-17, 0.5000000000000019984, 0.8660254037844375974 ) ) ;
#5656 = CARTESIAN_POINT ( 'NONE',  ( -1.582370436562975380, 4.859920694388930151, -4.019399823475544586 ) ) ;
#5657 = CIRCLE ( 'NONE', #6370, 2.375000000000000000 ) ;
#5658 = EDGE_LOOP ( 'NONE', ( #4698, #586, #3202, #13100, #11887 ) ) ;
#5659 = VECTOR ( 'NONE', #5484, 1000.000000000000114 ) ;
#5660 = LINE ( 'NONE', #3631, #8891 ) ;
#5661 = EDGE_LOOP ( 'NONE', ( #10429, #2183, #5228, #11184 ) ) ;
#5662 = CARTESIAN_POINT ( 'NONE',  ( 22.00000000000000000, 78.00000000000000000, 25.00000000000000000 ) ) ;
#5663 = FACE_OUTER_BOUND ( 'NONE', #4511, .T. ) ;
#5664 = EDGE_CURVE ( 'NONE', #641, #2625, #14044, .T. ) ;
#5665 = VERTEX_POINT ( 'NONE', #11027 ) ;
#5666 = CIRCLE ( 'NONE', #13875, 5.000000000000004441 ) ;
#5667 = ORIENTED_EDGE ( 'NONE', *, *, #2431, .F. ) ;
#5668 = AXIS2_PLACEMENT_3D ( 'NONE', #4730, #12540, #10271 ) ;
#5669 = VERTEX_POINT ( 'NONE', #11243 ) ;
#5670 = CARTESIAN_POINT ( 'NONE',  ( 4.871660775260041376, -3.916561903058248806, -1.361048636879858664 ) ) ;
#5671 = ORIENTED_EDGE ( 'NONE', *, *, #163, .F. ) ;
#5672 = CARTESIAN_POINT ( 'NONE',  ( 3.958476099524994130, -1.406653531809710644, -3.499999999999992895 ) ) ;
#5673 = CIRCLE ( 'NONE', #13881, 2.500000000000002220 ) ;
#5674 = CARTESIAN_POINT ( 'NONE',  ( 5.733169058567799681, -6.938893903907228378E-15, 0.000000000000000000 ) ) ;
#5675 = CARTESIAN_POINT ( 'NONE',  ( 0.3126073911696169993, 4.041451884327390331, 0.000000000000000000 ) ) ;
#5676 = CARTESIAN_POINT ( 'NONE',  ( 0.000000000000000000, 0.000000000000000000, -4.674599999999973221 ) ) ;
#5677 = CARTESIAN_POINT ( 'NONE',  ( -3.000000000000000000, -1.322063213371142838E-16, 2.400000000000013234 ) ) ;
#5678 = PRODUCT_DEFINITION_FORMATION_WITH_SPECIFIED_SOURCE ( 'ANY', '', #13505, .NOT_KNOWN. ) ;
#5679 = CARTESIAN_POINT ( 'NONE',  ( -108.6817075744281595, 69.57655509336026967, -3.299999999999976730 ) ) ;
#5680 = CARTESIAN_POINT ( 'NONE',  ( 4.158921614371304365, -1.986121848748764851, 3.559936047944501247 ) ) ;
#5681 = EDGE_CURVE ( 'NONE', #3192, #11427, #4467, .T. ) ;
#5682 = EDGE_CURVE ( 'NONE', #7559, #13013, #7195, .T. ) ;
#5683 = CARTESIAN_POINT ( 'NONE',  ( 20.00000000000000711, 20.00000000000000355, -25.00000000000000000 ) ) ;
#5684 = VECTOR ( 'NONE', #13740, 1000.000000000000000 ) ;
#5685 = EDGE_LOOP ( 'NONE', ( #4272, #14100, #13025, #8572 ) ) ;
#5686 = CARTESIAN_POINT ( 'NONE',  ( -1.360615521533644401, 4.061278559078192352, -3.205052026701860513 ) ) ;
#5687 = VERTEX_POINT ( 'NONE', #10283 ) ;
#5688 = CARTESIAN_POINT ( 'NONE',  ( 3.060208875726633249, -4.280211771583999791, -4.357749648769123851 ) ) ;
#5689 = DIRECTION ( 'NONE',  ( -0.000000000000000000, -0.000000000000000000, 1.000000000000000000 ) ) ;
#5690 = CARTESIAN_POINT ( 'NONE',  ( -5.000000000000000000, -2.094342041905651541, -4.137519424005751567 ) ) ;
#5691 = PLANE ( 'NONE',  #7957 ) ;
#5692 = FACE_OUTER_BOUND ( 'NONE', #5984, .T. ) ;
#5693 = FACE_OUTER_BOUND ( 'NONE', #13459, .T. ) ;
#5694 = LINE ( 'NONE', #154, #9376 ) ;
#5695 = ORIENTED_EDGE ( 'NONE', *, *, #3496, .F. ) ;
#5696 = DIRECTION ( 'NONE',  ( -1.000000000000000000, -0.000000000000000000, -0.000000000000000000 ) ) ;
#5697 = EDGE_LOOP ( 'NONE', ( #4829, #6409 ) ) ;
#5698 = EDGE_LOOP ( 'NONE', ( #2057, #5573, #12944, #5970 ) ) ;
#5699 = ORIENTED_EDGE ( 'NONE', *, *, #4516, .T. ) ;
#5700 = CLOSED_SHELL ( 'NONE', ( #123, #9823, #12280, #8861, #13095, #1809, #8687, #6435, #11113, #5725, #11522, #6285, #3040, #4785, #8898, #4404, #1446, #2997, #736, #14155, #5393, #9502, #6232, #7351, #3280, #9273, #9038, #6847, #8187, #3039, #12190, #5990, #7668, #8107, #11634, #7039, #6891, #1909, #11294, #3789, #14110, #13799, #12065, #11354 ) ) ;
#5701 = DIRECTION ( 'NONE',  ( -1.000000000000000000, 0.000000000000000000, 0.000000000000000000 ) ) ;
#5702 = FACE_OUTER_BOUND ( 'NONE', #11575, .T. ) ;
#5703 = DIRECTION ( 'NONE',  ( 0.000000000000000000, 0.000000000000000000, 1.000000000000000000 ) ) ;
#5704 = ORIENTED_EDGE ( 'NONE', *, *, #10484, .F. ) ;
#5705 = DIRECTION ( 'NONE',  ( 1.913084959030911013E-15, -1.000000000000000000, 0.000000000000000000 ) ) ;
#5706 = ADVANCED_FACE ( 'NONE', ( #11530 ), #1357, .T. ) ;
#5707 =( NAMED_UNIT ( * ) SI_UNIT ( $, .STERADIAN. ) SOLID_ANGLE_UNIT ( ) );
#5708 = ADVANCED_FACE ( 'NONE', ( #12703 ), #9412, .T. ) ;
#5709 = ORIENTED_EDGE ( 'NONE', *, *, #2064, .T. ) ;
#5710 = CARTESIAN_POINT ( 'NONE',  ( 20.00000000000000355, 17.00000000000000000, -25.00000000000000000 ) ) ;
#5711 = ORIENTED_EDGE ( 'NONE', *, *, #8453, .F. ) ;
#5712 = CARTESIAN_POINT ( 'NONE',  ( -13.00000000000000533, 24.50000000000001421, 0.000000000000000000 ) ) ;
#5713 = CARTESIAN_POINT ( 'NONE',  ( -129.3408537872145132, 189.5765550933606107, -13.99999999999998401 ) ) ;
#5714 = CARTESIAN_POINT ( 'NONE',  ( -4.185558440016327708, -3.356969399843937385, -0.2680587191991219975 ) ) ;
#5715 = CARTESIAN_POINT ( 'NONE',  ( 5.599999999999994316, 4.041451884327390331, 0.000000000000000000 ) ) ;
#5716 = DIRECTION ( 'NONE',  ( 2.312964634635743943E-16, 1.000000000000000000, 0.000000000000000000 ) ) ;
#5717 = EDGE_CURVE ( 'NONE', #11894, #1315, #13167, .T. ) ;
#5718 = CARTESIAN_POINT ( 'NONE',  ( 0.1702248550645398539, 5.871782057790552400, -4.589066185948675880 ) ) ;
#5719 = CARTESIAN_POINT ( 'NONE',  ( 1.560000000000005826, 1.732050807568871864, 0.000000000000000000 ) ) ;
#5720 = EDGE_LOOP ( 'NONE', ( #12901, #7725, #3398, #14421 ) ) ;
#5721 = CYLINDRICAL_SURFACE ( 'NONE', #7165, 2.500000000000002220 ) ;
#5722 = EDGE_CURVE ( 'NONE', #192, #13539, #8645, .T. ) ;
#5723 = ORIENTED_EDGE ( 'NONE', *, *, #2770, .T. ) ;
#5724 = CARTESIAN_POINT ( 'NONE',  ( -118.6817075744281595, 69.57655509336025546, 0.000000000000000000 ) ) ;
#5725 = ADVANCED_FACE ( 'NONE', ( #273 ), #2765, .F. ) ;
#5726 = ORIENTED_EDGE ( 'NONE', *, *, #13402, .F. ) ;
#5727 = ORIENTED_EDGE ( 'NONE', *, *, #12789, .T. ) ;
#5728 = ORIENTED_EDGE ( 'NONE', *, *, #5717, .T. ) ;
#5729 = CARTESIAN_POINT ( 'NONE',  ( 22.00000000000000000, 57.00000000000000000, -25.00000000000000000 ) ) ;
#5730 = CARTESIAN_POINT ( 'NONE',  ( 88.22284556172391490, -83.66032599071898801, 28.00000000000000000 ) ) ;
#5731 = DIRECTION ( 'NONE',  ( -1.000000000000000000, 0.000000000000000000, 0.000000000000000000 ) ) ;
#5732 = CARTESIAN_POINT ( 'NONE',  ( 22.00000000000000355, 37.00000000000000711, -25.00000000000000000 ) ) ;
#5733 = EDGE_CURVE ( 'NONE', #1722, #5395, #3646, .T. ) ;
#5734 = CARTESIAN_POINT ( 'NONE',  ( 5.599999999999994316, 2.020725942163681399, -3.499999999999996003 ) ) ;
#5735 = ORIENTED_EDGE ( 'NONE', *, *, #11672, .F. ) ;
#5736 = CARTESIAN_POINT ( 'NONE',  ( 0.000000000000000000, 0.000000000000000000, 25.00000000000000000 ) ) ;
#5737 = LINE ( 'NONE', #12627, #941 ) ;
#5738 = DIRECTION ( 'NONE',  ( -1.000000000000000000, 0.000000000000000000, 0.000000000000000000 ) ) ;
#5739 = CARTESIAN_POINT ( 'NONE',  ( 31.24550000000003536, 0.000000000000000000, 0.000000000000000000 ) ) ;
#5740 = AXIS2_PLACEMENT_3D ( 'NONE', #5503, #961, #11136 ) ;
#5741 = ORIENTED_EDGE ( 'NONE', *, *, #8752, .T. ) ;
#5742 = ORIENTED_EDGE ( 'NONE', *, *, #5255, .T. ) ;
#5743 = LINE ( 'NONE', #210, #2663 ) ;
#5744 = ORIENTED_EDGE ( 'NONE', *, *, #5650, .T. ) ;
#5745 = EDGE_LOOP ( 'NONE', ( #7096, #7157, #8311, #4477 ) ) ;
#5746 = DIRECTION ( 'NONE',  ( 0.000000000000000000, 0.000000000000000000, 1.000000000000000000 ) ) ;
#5747 = VECTOR ( 'NONE', #5936, 1000.000000000000227 ) ;
#5748 = CARTESIAN_POINT ( 'NONE',  ( 0.1388410611046012044, -2.351840044243032057, 2.926493552096011364 ) ) ;
#5749 = CARTESIAN_POINT ( 'NONE',  ( -31.44014396567295577, 21.68342561534834445, 8.000000000000007105 ) ) ;
#5750 =( REPRESENTATION_RELATIONSHIP ('NONE','NONE', #10295, #11805 ) REPRESENTATION_RELATIONSHIP_WITH_TRANSFORMATION ( #7877 )SHAPE_REPRESENTATION_RELATIONSHIP( ) );
#5751 = ADVANCED_FACE ( 'NONE', ( #1288 ), #12162, .T. ) ;
#5752 = CYLINDRICAL_SURFACE ( 'NONE', #1424, 2.600000000000004974 ) ;
#5753 = VECTOR ( 'NONE', #11590, 1000.000000000000000 ) ;
#5754 = ORIENTED_EDGE ( 'NONE', *, *, #8528, .F. ) ;
#5755 = DIRECTION ( 'NONE',  ( -1.000000000000000000, -3.286707217423839940E-17, -2.273843122241288053E-18 ) ) ;
#5756 = AXIS2_PLACEMENT_3D ( 'NONE', #6192, #13895, #9415 ) ;
#5757 = CARTESIAN_POINT ( 'NONE',  ( -129.3408537872145132, 189.5765550933606107, -13.99999999999998401 ) ) ;
#5758 = EDGE_LOOP ( 'NONE', ( #10144, #11076, #1754, #6948 ) ) ;
#5759 = PRODUCT_DEFINITION_SHAPE ( 'NONE', 'NONE',  #2574 ) ;
#5760 = VERTEX_POINT ( 'NONE', #10430 ) ;
#5761 = DIRECTION ( 'NONE',  ( 1.723842398015259277E-15, -1.000000000000000000, 0.000000000000000000 ) ) ;
#5762 = AXIS2_PLACEMENT_3D ( 'NONE', #6523, #2010, #6450 ) ;
#5763 = AXIS2_PLACEMENT_3D ( 'NONE', #4809, #10153, #6917 ) ;
#5764 = ORIENTED_EDGE ( 'NONE', *, *, #1851, .T. ) ;
#5765 = ORIENTED_EDGE ( 'NONE', *, *, #13086, .F. ) ;
#5766 = CARTESIAN_POINT ( 'NONE',  ( 4.962664318264591756, -2.733102959025379253, 3.415681285063929984 ) ) ;
#5767 = DIRECTION ( 'NONE',  ( 0.000000000000000000, 0.000000000000000000, 1.000000000000000000 ) ) ;
#5768 = ADVANCED_FACE ( 'NONE', ( #2692 ), #193, .T. ) ;
#5769 = EDGE_CURVE ( 'NONE', #3428, #1985, #10765, .T. ) ;
#5770 =( NAMED_UNIT ( * ) PLANE_ANGLE_UNIT ( ) SI_UNIT ( $, .RADIAN. ) );
#5771 = AXIS2_PLACEMENT_3D ( 'NONE', #3317, #14365, #2059 ) ;
#5772 = AXIS2_PLACEMENT_3D ( 'NONE', #8674, #6463, #12333 ) ;
#5773 = VECTOR ( 'NONE', #13586, 1000.000000000000000 ) ;
#5774 = ORIENTED_EDGE ( 'NONE', *, *, #13636, .F. ) ;
#5775 = ORIENTED_EDGE ( 'NONE', *, *, #2090, .T. ) ;
#5776 = DIRECTION ( 'NONE',  ( 1.000000000000000000, 0.000000000000000000, 0.000000000000000000 ) ) ;
#5777 = FACE_OUTER_BOUND ( 'NONE', #3316, .T. ) ;
#5778 = ORIENTED_EDGE ( 'NONE', *, *, #4034, .F. ) ;
#5779 = DIRECTION ( 'NONE',  ( 0.000000000000000000, 4.440892098500620738E-16, 1.000000000000000000 ) ) ;
#5780 = COLOUR_RGB ( '', 0.08235294, 0.09019608, 0.10196078) ;
#5781 = CARTESIAN_POINT ( 'NONE',  ( -0.4022569922705768186, 5.541259509125445071, -0.4198507760575658776 ) ) ;
#5782 = CARTESIAN_POINT ( 'NONE',  ( 4.114405500665253790, 2.025575754679707075, 3.508400121684931428 ) ) ;
#5783 = VERTEX_POINT ( 'NONE', #4805 ) ;
#5784 = FACE_OUTER_BOUND ( 'NONE', #9759, .T. ) ;
#5785 = CARTESIAN_POINT ( 'NONE',  ( 2.750000000000002665, 0.000000000000000000, 4.750000000000000000 ) ) ;
#5786 = CARTESIAN_POINT ( 'NONE',  ( 5.560781378645534900, 9.260561282218635514E-16, -3.699999999999981082 ) ) ;
#5787 = DIRECTION ( 'NONE',  ( -0.000000000000000000, -1.000000000000000000, 0.000000000000000000 ) ) ;
#5788 = LINE ( 'NONE', #13803, #12630 ) ;
#5789 = ORIENTED_EDGE ( 'NONE', *, *, #13199, .F. ) ;
#5790 = DIRECTION ( 'NONE',  ( -1.000000000000000000, -1.224646799147353454E-16, 0.000000000000000000 ) ) ;
#5791 = VECTOR ( 'NONE', #12844, 1000.000000000000000 ) ;
#5792 = DIRECTION ( 'NONE',  ( 1.000000000000000000, 0.000000000000000000, 0.000000000000000000 ) ) ;
#5793 = ORIENTED_EDGE ( 'NONE', *, *, #3321, .T. ) ;
#5794 = PLANE ( 'NONE',  #11865 ) ;
#5795 = CIRCLE ( 'NONE', #14021, 16.00000000000001421 ) ;
#5796 = ORIENTED_EDGE ( 'NONE', *, *, #13715, .F. ) ;
#5797 = ORIENTED_EDGE ( 'NONE', *, *, #2348, .T. ) ;
#5798 = ORIENTED_EDGE ( 'NONE', *, *, #987, .T. ) ;
#5799 = DIRECTION ( 'NONE',  ( -1.000000000000000000, 0.000000000000000000, 0.000000000000000000 ) ) ;
#5800 = DIRECTION ( 'NONE',  ( 1.000000000000000000, -0.000000000000000000, -0.000000000000000000 ) ) ;
#5801 = CARTESIAN_POINT ( 'NONE',  ( 32.50229726637438432, 120.2985749985466839, 25.00000000000000000 ) ) ;
#5802 = AXIS2_PLACEMENT_3D ( 'NONE', #9902, #3329, #2003 ) ;
#5803 = ADVANCED_FACE ( 'NONE', ( #9260 ), #8155, .F. ) ;
#5804 = CARTESIAN_POINT ( 'NONE',  ( 78.52142056027061301, -86.08568224108226730, 33.00000000000000000 ) ) ;
#5805 = ADVANCED_FACE ( 'NONE', ( #3576 ), #7130, .T. ) ;
#5806 = CARTESIAN_POINT ( 'NONE',  ( 32.60000000000000142, 29.99999999999999645, -34.50000000000000000 ) ) ;
#5807 = VERTEX_POINT ( 'NONE', #13744 ) ;
#5808 = CARTESIAN_POINT ( 'NONE',  ( 47.05443476855437268, 62.09002498982675888, -25.00000000000000000 ) ) ;
#5809 = AXIS2_PLACEMENT_3D ( 'NONE', #5470, #11925, #8829 ) ;
#5810 = DIRECTION ( 'NONE',  ( -0.000000000000000000, -0.000000000000000000, -1.000000000000000000 ) ) ;
#5811 = DIRECTION ( 'NONE',  ( 1.000000000000000000, 0.000000000000000000, 0.000000000000000000 ) ) ;
#5812 = DIRECTION ( 'NONE',  ( 1.892425610156516875E-16, 1.000000000000000000, 0.000000000000000000 ) ) ;
#5813 = VECTOR ( 'NONE', #10988, 1000.000000000000000 ) ;
#5814 = EDGE_CURVE ( 'NONE', #8390, #13637, #4920, .T. ) ;
#5815 = ORIENTED_EDGE ( 'NONE', *, *, #7480, .T. ) ;
#5816 = CARTESIAN_POINT ( 'NONE',  ( -4.175647895129166898, 2.207990717223085486, -3.169390900447837112 ) ) ;
#5817 = ORIENTED_EDGE ( 'NONE', *, *, #1343, .T. ) ;
#5818 = DIRECTION ( 'NONE',  ( -0.8571673007021134438, 0.000000000000000000, -0.5150380749100522682 ) ) ;
#5819 = EDGE_CURVE ( 'NONE', #3492, #2629, #573, .T. ) ;
#5820 = CARTESIAN_POINT ( 'NONE',  ( 5.103531824934171013, 2.354098498486459246, -4.077418205400141105 ) ) ;
#5821 = FACE_OUTER_BOUND ( 'NONE', #1618, .T. ) ;
#5822 = CARTESIAN_POINT ( 'NONE',  ( 33.99999999999998579, 80.00000000000000000, -25.00000000000000000 ) ) ;
#5823 = PRESENTATION_LAYER_ASSIGNMENT (  '', '', ( #11223 ) ) ;
#5824 = VERTEX_POINT ( 'NONE', #11761 ) ;
#5825 = AXIS2_PLACEMENT_3D ( 'NONE', #8954, #13444, #1204 ) ;
#5826 = CYLINDRICAL_SURFACE ( 'NONE', #8197, 2.500000000000002220 ) ;
#5827 = DIRECTION ( 'NONE',  ( -0.8191520442889909104, 4.865168473767738639E-47, -0.5735764363510472696 ) ) ;
#5828 = CARTESIAN_POINT ( 'NONE',  ( 4.000000000000003553, 2.309401076758501592, -4.699999999999981526 ) ) ;
#5829 = EDGE_LOOP ( 'NONE', ( #11775, #10763, #8742, #10420 ) ) ;
#5830 = EDGE_CURVE ( 'NONE', #12564, #14306, #3062, .T. ) ;
#5831 = CIRCLE ( 'NONE', #12168, 2.500000000000000444 ) ;
#5832 = ORIENTED_EDGE ( 'NONE', *, *, #1775, .F. ) ;
#5833 = APPLICATION_CONTEXT ( 'automotive_design' ) ;
#5834 = PRODUCT_DEFINITION_CONTEXT ( 'detailed design', #10632, 'design' ) ;
#5836 = ORIENTED_EDGE ( 'NONE', *, *, #5890, .T. ) ;
#5835 = AXIS2_PLACEMENT_3D ( 'NONE', #11593, #9253, #6100 ) ;
#5837 = CARTESIAN_POINT ( 'NONE',  ( -1.533718260776178309E-15, -5.773502691896303496, -4.369522543421428651 ) ) ;
#5838 = CARTESIAN_POINT ( 'NONE',  ( 1.560000000000005826, 0.000000000000000000, 0.000000000000000000 ) ) ;
#5839 = VECTOR ( 'NONE', #7892, 1000.000000000000000 ) ;
#5840 = SURFACE_STYLE_FILL_AREA ( #13567 ) ;
#5841 = EDGE_LOOP ( 'NONE', ( #6121, #1024, #6748, #13725 ) ) ;
#5842 =( GEOMETRIC_REPRESENTATION_CONTEXT ( 3 ) GLOBAL_UNCERTAINTY_ASSIGNED_CONTEXT ( ( #11880 ) ) GLOBAL_UNIT_ASSIGNED_CONTEXT ( ( #814, #10768, #3031 ) ) REPRESENTATION_CONTEXT ( 'NONE', 'WORKASPACE' ) );
#5843 = AXIS2_PLACEMENT_3D ( 'NONE', #10757, #14139, #10894 ) ;
#5844 = ORIENTED_EDGE ( 'NONE', *, *, #7715, .T. ) ;
#5845 = CARTESIAN_POINT ( 'NONE',  ( 34.92765351673772045, 110.5971499970933536, 25.00000000000000000 ) ) ;
#5846 = VECTOR ( 'NONE', #6884, 1000.000000000000000 ) ;
#5847 = CARTESIAN_POINT ( 'NONE',  ( 5.035982117295162652, 2.314736229921479094, -4.009240756344450318 ) ) ;
#5848 = ORIENTED_EDGE ( 'NONE', *, *, #3777, .F. ) ;
#5849 = EDGE_CURVE ( 'NONE', #5508, #6997, #5026, .T. ) ;
#5850 = DIRECTION ( 'NONE',  ( -1.000000000000000000, 0.000000000000000000, 0.000000000000000000 ) ) ;
#5851 = EDGE_CURVE ( 'NONE', #14160, #4271, #6842, .T. ) ;
#5852 = VERTEX_POINT ( 'NONE', #11980 ) ;
#5853 = AXIS2_PLACEMENT_3D ( 'NONE', #598, #3016, #8554 ) ;
#5854 = VECTOR ( 'NONE', #10893, 1000.000000000000000 ) ;
#5855 = PLANE ( 'NONE',  #12714 ) ;
#5856 = CARTESIAN_POINT ( 'NONE',  ( 28.00000000000000355, 29.99999999999999645, -34.50000000000000000 ) ) ;
#5857 = EDGE_LOOP ( 'NONE', ( #3976, #13238, #14079, #11487, #9948, #4620, #10499, #9014, #3521, #11903, #10867, #6840 ) ) ;
#5858 = DIRECTION ( 'NONE',  ( -1.000000000000000000, 0.000000000000000000, 0.000000000000000000 ) ) ;
#5859 = CARTESIAN_POINT ( 'NONE',  ( 0.000000000000000000, 0.000000000000000000, 0.000000000000000000 ) ) ;
#5860 = CARTESIAN_POINT ( 'NONE',  ( -118.6817075744282306, 109.5765550933602697, 0.000000000000000000 ) ) ;
#5861 = ORIENTED_EDGE ( 'NONE', *, *, #4348, .T. ) ;
#5862 = FACE_OUTER_BOUND ( 'NONE', #8800, .T. ) ;
#5863 = VERTEX_POINT ( 'NONE', #1955 ) ;
#5864 = AXIS2_PLACEMENT_3D ( 'NONE', #8298, #2840, #12549 ) ;
#5865 = CARTESIAN_POINT ( 'NONE',  ( 44.70372226782771463, 81.49287499273339108, 25.00000000000000000 ) ) ;
#5866 = AXIS2_PLACEMENT_3D ( 'NONE', #461, #4915, #9379 ) ;
#5867 = CIRCLE ( 'NONE', #9366, 5.000000000000004441 ) ;
#5868 = CARTESIAN_POINT ( 'NONE',  ( 0.000000000000000000, 0.000000000000000000, 0.000000000000000000 ) ) ;
#5869 = ORIENTED_EDGE ( 'NONE', *, *, #13068, .T. ) ;
#5870 = DIRECTION ( 'NONE',  ( 1.000000000000000000, 0.000000000000000000, 0.000000000000000000 ) ) ;
#5871 = EDGE_CURVE ( 'NONE', #3920, #3697, #2828, .T. ) ;
#5872 = EDGE_LOOP ( 'NONE', ( #541, #6769, #14123 ) ) ;
#5873 = CARTESIAN_POINT ( 'NONE',  ( 5.024612689793150899, 4.625309484956555472, 0.000000000000000000 ) ) ;
#5874 = ORIENTED_EDGE ( 'NONE', *, *, #12278, .F. ) ;
#5875 = ORIENTED_EDGE ( 'NONE', *, *, #12402, .T. ) ;
#5876 = CARTESIAN_POINT ( 'NONE',  ( 2.750000000000003553, 40.49999999999999289, 0.000000000000000000 ) ) ;
#5877 = CARTESIAN_POINT ( 'NONE',  ( -1.050836307075461606, 48.43494986415684878, 7.868526909826536020 ) ) ;
#5878 =( BOUNDED_SURFACE ( )  B_SPLINE_SURFACE ( 3, 2, ( 
 ( #10159, #142, #4941 ),
 ( #11669, #4797, #10502 ),
 ( #9482, #9557, #11521 ),
 ( #3927, #8371, #14034 ),
 ( #9402, #12849, #10654 ),
 ( #13884, #2601, #3859 ) ),
 .UNSPECIFIED., .F., .F., .F. ) 
 B_SPLINE_SURFACE_WITH_KNOTS ( ( 4, 2, 4 ),
 ( 3, 3 ),
 ( 0.01886032586153035123, 0.02121253401777978276, 0.02356474217402921081 ),
 ( 0.000000000000000000, 1.000000000000000000 ),
 .UNSPECIFIED. ) 
 GEOMETRIC_REPRESENTATION_ITEM ( )  RATIONAL_B_SPLINE_SURFACE ( (
 ( 1.000000000000000000, 0.8047781103519388024, 1.000000000000000000),
 ( 1.000000000000000000, 0.8123785825777287695, 1.000000000000000000),
 ( 1.000000000000000000, 0.8190671539558022074, 1.000000000000000000),
 ( 1.000000000000000000, 0.8192352255065119548, 1.000000000000000000),
 ( 1.000000000000000000, 0.8126129677038673726, 1.000000000000000000),
 ( 1.000000000000000000, 0.8047712537969721192, 1.000000000000000000) ) ) 
 REPRESENTATION_ITEM ( '' )  SURFACE ( )  );
#5879 = STYLED_ITEM ( 'NONE', ( #13210 ), #10106 ) ;
#5880 = EDGE_LOOP ( 'NONE', ( #1321, #11724, #920, #11834 ) ) ;
#5881 = EDGE_CURVE ( 'NONE', #11189, #780, #8881, .T. ) ;
#5882 = DIRECTION ( 'NONE',  ( 0.000000000000000000, 0.000000000000000000, -1.000000000000000000 ) ) ;
#5883 = VECTOR ( 'NONE', #11483, 1000.000000000000000 ) ;
#5884 = AXIS2_PLACEMENT_3D ( 'NONE', #6366, #3968, #7454 ) ;
#5885 = DIRECTION ( 'NONE',  ( 0.000000000000000000, 0.000000000000000000, 1.000000000000000000 ) ) ;
#5886 = LINE ( 'NONE', #11384, #4644 ) ;
#5887 = CARTESIAN_POINT ( 'NONE',  ( 21.68170757442808849, 141.2731697022877313, -23.00000000000000000 ) ) ;
#5888 = LINE ( 'NONE', #13685, #7711 ) ;
#5889 = ITEM_DEFINED_TRANSFORMATION ( 'NONE', 'NONE', #1732,  #11025 ) ;
#5890 = EDGE_CURVE ( 'NONE', #8562, #4098, #647, .T. ) ;
#5891 = DIRECTION ( 'NONE',  ( 0.000000000000000000, 0.000000000000000000, -1.000000000000000000 ) ) ;
#5892 = CARTESIAN_POINT ( 'NONE',  ( -5.551115123125782702E-14, 3.464101615137750390, -2.000000000000001776 ) ) ;
#5893 = CARTESIAN_POINT ( 'NONE',  ( 20.00000000000000000, 47.00000000000000000, -25.00000000000000000 ) ) ;
#5894 = CARTESIAN_POINT ( 'NONE',  ( 13.00000000000000533, 29.99999999999999289, 8.000000000000007105 ) ) ;
#5895 = VECTOR ( 'NONE', #2082, 1000.000000000000000 ) ;
#5896 = EDGE_CURVE ( 'NONE', #8969, #5220, #8182, .T. ) ;
#5897 = ORIENTED_EDGE ( 'NONE', *, *, #3402, .T. ) ;
#5898 = CARTESIAN_POINT ( 'NONE',  ( -3.436326524993375209, 2.634838109288609509, -3.231543764078446568 ) ) ;
#5899 = ORIENTED_EDGE ( 'NONE', *, *, #9224, .T. ) ;
#5900 = PLANE ( 'NONE',  #464 ) ;
#5901 = CARTESIAN_POINT ( 'NONE',  ( 39.85300976710104948, 100.8957249956400375, 25.00000000000000000 ) ) ;
#5902 = CARTESIAN_POINT ( 'NONE',  ( -5.244721914230359161, -2.047008728252464937, -4.475704751401925030 ) ) ;
#5903 = CARTESIAN_POINT ( 'NONE',  ( -118.6817075744282306, 109.5765550933602697, 3.299999999999976730 ) ) ;
#5904 = VECTOR ( 'NONE', #5063, 1000.000000000000114 ) ;
#5905 = ORIENTED_EDGE ( 'NONE', *, *, #13529, .F. ) ;
#5906 = CARTESIAN_POINT ( 'NONE',  ( 0.3126073911696169993, 2.020725942163681399, 3.499999999999996003 ) ) ;
#5907 = CARTESIAN_POINT ( 'NONE',  ( -1.343349931607518297E-17, 40.49999999999999289, -22.25000000000000000 ) ) ;
#5908 = CARTESIAN_POINT ( 'NONE',  ( 4.870911883258405517, 0.7936069845605383533, 4.072347588220287307 ) ) ;
#5909 = ADVANCED_FACE ( 'NONE', ( #6106 ), #10860, .F. ) ;
#5910 = CARTESIAN_POINT ( 'NONE',  ( 0.6507732100473498926, -4.243078065514795938, -0.2236248678334991080 ) ) ;
#5911 = VECTOR ( 'NONE', #587, 1000.000000000000227 ) ;
#5912 = CARTESIAN_POINT ( 'NONE',  ( 0.000000000000000000, 0.000000000000000000, 0.000000000000000000 ) ) ;
#5913 = EDGE_CURVE ( 'NONE', #2320, #10194, #7238, .T. ) ;
#5914 = ORIENTED_EDGE ( 'NONE', *, *, #1266, .F. ) ;
#5915 = MECHANICAL_DESIGN_GEOMETRIC_PRESENTATION_REPRESENTATION (  '', ( #12250 ), #3381 ) ;
#5916 = VERTEX_POINT ( 'NONE', #13294 ) ;
#5917 = ORIENTED_EDGE ( 'NONE', *, *, #4090, .T. ) ;
#5918 = VECTOR ( 'NONE', #6103, 1000.000000000000000 ) ;
#5919 = DIRECTION ( 'NONE',  ( 0.000000000000000000, 0.000000000000000000, -1.000000000000000000 ) ) ;
#5920 = CARTESIAN_POINT ( 'NONE',  ( 0.000000000000000000, 40.49999999999999289, 8.000000000000007105 ) ) ;
#5921 = SURFACE_STYLE_FILL_AREA ( #1544 ) ;
#5922 = PLANE ( 'NONE',  #4712 ) ;
#5923 = EDGE_CURVE ( 'NONE', #4098, #1181, #934, .T. ) ;
#5924 = ORIENTED_EDGE ( 'NONE', *, *, #13950, .T. ) ;
#5925 = DIRECTION ( 'NONE',  ( 0.000000000000000000, 0.000000000000000000, -1.000000000000000000 ) ) ;
#5926 = CARTESIAN_POINT ( 'NONE',  ( 5.056385618527004411, 2.321455725013334082, -4.020879263244736990 ) ) ;
#5927 = ORIENTED_EDGE ( 'NONE', *, *, #225, .T. ) ;
#5928 = EDGE_CURVE ( 'NONE', #10936, #6145, #6535, .T. ) ;
#5929 = FACE_OUTER_BOUND ( 'NONE', #9836, .T. ) ;
#5930 = EDGE_LOOP ( 'NONE', ( #4795, #6999 ) ) ;
#5931 = VERTEX_POINT ( 'NONE', #11007 ) ;
#5932 = DIRECTION ( 'NONE',  ( 0.000000000000000000, 0.000000000000000000, -1.000000000000000000 ) ) ;
#5933 = DIRECTION ( 'NONE',  ( 0.000000000000000000, 0.000000000000000000, -1.000000000000000000 ) ) ;
#5934 = CARTESIAN_POINT ( 'NONE',  ( 4.082498951862934433, -2.020725942163681399, -3.500000000000010214 ) ) ;
#5935 = CARTESIAN_POINT ( 'NONE',  ( 5.085009278891528872, 2.385862568036605680, -4.000000000000002665 ) ) ;
#5936 = DIRECTION ( 'NONE',  ( -0.2425356250363328581, 0.9701425001453318764, 0.000000000000000000 ) ) ;
#5937 = ADVANCED_FACE ( 'NONE', ( #5449 ), #3755, .F. ) ;
#5938 = CARTESIAN_POINT ( 'NONE',  ( 78.52142056027061301, -86.08568224108226730, -28.00000000000000000 ) ) ;
#5939 = EDGE_LOOP ( 'NONE', ( #9272, #4933, #971, #5442 ) ) ;
#5940 = DIRECTION ( 'NONE',  ( 0.000000000000000000, 0.000000000000000000, 1.000000000000000000 ) ) ;
#5941 = EDGE_LOOP ( 'NONE', ( #3079, #4114, #527 ) ) ;
#5942 = LINE ( 'NONE', #4859, #12830 ) ;
#5943 = CARTESIAN_POINT ( 'NONE',  ( -3.999999999999996447, 2.309401076758494487, -4.699999999999981526 ) ) ;
#5944 = ORIENTED_EDGE ( 'NONE', *, *, #10036, .F. ) ;
#5945 = DIRECTION ( 'NONE',  ( 0.000000000000000000, 0.000000000000000000, 1.000000000000000000 ) ) ;
#5946 = PLANE ( 'NONE',  #12231 ) ;
#5947 = ORIENTED_EDGE ( 'NONE', *, *, #499, .F. ) ;
#5948 =( REPRESENTATION_RELATIONSHIP ('NONE','NONE', #10295, #7856 ) REPRESENTATION_RELATIONSHIP_WITH_TRANSFORMATION ( #1293 )SHAPE_REPRESENTATION_RELATIONSHIP( ) );
#5949 = CARTESIAN_POINT ( 'NONE',  ( 20.00000000000000355, 50.00000000000000000, -25.00000000000000000 ) ) ;
#5950 = ORIENTED_EDGE ( 'NONE', *, *, #7239, .T. ) ;
#5951 = ORIENTED_EDGE ( 'NONE', *, *, #299, .F. ) ;
#5952 = FACE_OUTER_BOUND ( 'NONE', #2492, .T. ) ;
#5953 = CARTESIAN_POINT ( 'NONE',  ( -2.650472254991408150, 48.05066328782152851, 7.006789553262803949 ) ) ;
#5954 = CARTESIAN_POINT ( 'NONE',  ( 4.000000000000003553, 2.309401076758501592, -4.699999999999981526 ) ) ;
#5955 = DIRECTION ( 'NONE',  ( 1.000000000000000000, 0.000000000000000000, 0.000000000000000000 ) ) ;
#5956 = DIRECTION ( 'NONE',  ( -0.000000000000000000, -1.000000000000000000, 0.000000000000000000 ) ) ;
#5957 = EDGE_CURVE ( 'NONE', #5614, #1344, #115, .T. ) ;
#5958 = CARTESIAN_POINT ( 'NONE',  ( 59.91362529070399034, 29.57655509336062849, 28.00000000000000000 ) ) ;
#5959 = EDGE_CURVE ( 'NONE', #10361, #10652, #12332, .T. ) ;
#5960 = SURFACE_STYLE_FILL_AREA ( #1518 ) ;
#5961 = CARTESIAN_POINT ( 'NONE',  ( 118.6817075744280316, 69.57655509336046862, 3.299999999999976730 ) ) ;
#5963 = VECTOR ( 'NONE', #11204, 1000.000000000000000 ) ;
#5962 = CARTESIAN_POINT ( 'NONE',  ( -3.999999999999991118, 1.677751148815752824, -3.235249634002968833 ) ) ;
#5964 = FACE_OUTER_BOUND ( 'NONE', #2201, .T. ) ;
#5965 = CARTESIAN_POINT ( 'NONE',  ( 1.503496978826011311E-15, 4.647089433458768681, -3.272167766733379946 ) ) ;
#5966 = ADVANCED_FACE ( 'NONE', ( #4586 ), #11407, .F. ) ;
#5967 = VERTEX_POINT ( 'NONE', #3416 ) ;
#5968 = CARTESIAN_POINT ( 'NONE',  ( -3.081487911019577365E-30, 3.469446951953614189E-15, -6.000000000000005329 ) ) ;
#5969 = ORIENTED_EDGE ( 'NONE', *, *, #5122, .T. ) ;
#5970 = ORIENTED_EDGE ( 'NONE', *, *, #13558, .F. ) ;
#5971 = DIRECTION ( 'NONE',  ( 1.000000000000000000, 0.000000000000000000, 0.000000000000000000 ) ) ;
#5972 = CARTESIAN_POINT ( 'NONE',  ( 0.02993401039713041584, -2.688325911136451030, 2.343682934607755897 ) ) ;
#5973 = LINE ( 'NONE', #10529, #11912 ) ;
#5974 = CARTESIAN_POINT ( 'NONE',  ( 27.75000000000001066, 0.000000000000000000, 2.055000000000000160 ) ) ;
#5975 = DIRECTION ( 'NONE',  ( 0.000000000000000000, 0.000000000000000000, -1.000000000000000000 ) ) ;
#5976 = ADVANCED_FACE ( 'NONE', ( #5377 ), #12187, .T. ) ;
#5977 = FACE_OUTER_BOUND ( 'NONE', #11655, .T. ) ;
#5978 = DIRECTION ( 'NONE',  ( 0.000000000000000000, 0.000000000000000000, -1.000000000000000000 ) ) ;
#5979 = CARTESIAN_POINT ( 'NONE',  ( 4.962672901883133036, 1.591562006530089723, 4.074777397737123330 ) ) ;
#5980 = CARTESIAN_POINT ( 'NONE',  ( -3.000000000000000888, 3.836840991697820422E-15, -25.03750572909319061 ) ) ;
#5981 = LINE ( 'NONE', #12580, #11274 ) ;
#5982 = ORIENTED_EDGE ( 'NONE', *, *, #6678, .T. ) ;
#5983 = VECTOR ( 'NONE', #2591, 1000.000000000000000 ) ;
#5984 = EDGE_LOOP ( 'NONE', ( #13991, #1228, #7284, #7010, #2277 ) ) ;
#5985 = PRODUCT_DEFINITION_CONTEXT ( 'detailed design', #3001, 'design' ) ;
#5986 = ORIENTED_EDGE ( 'NONE', *, *, #5570, .F. ) ;
#5987 = AXIS2_PLACEMENT_3D ( 'NONE', #2693, #13960, #4876 ) ;
#5988 = DIRECTION ( 'NONE',  ( -1.321694076934709169E-16, 1.000000000000000000, -0.000000000000000000 ) ) ;
#5989 = CARTESIAN_POINT ( 'NONE',  ( 4.175813232069169878, -2.061359961916378492, -3.570380186727409200 ) ) ;
#5990 = ADVANCED_FACE ( 'NONE', ( #12262 ), #9991, .T. ) ;
#5991 = EDGE_CURVE ( 'NONE', #1, #1219, #6537, .T. ) ;
#5992 = ORIENTED_EDGE ( 'NONE', *, *, #12112, .F. ) ;
#5993 = ADVANCED_FACE ( 'NONE', ( #5653 ), #11578, .F. ) ;
#5994 = CIRCLE ( 'NONE', #8102, 2.499999999999999112 ) ;
#5995 = DIRECTION ( 'NONE',  ( -1.000000000000000000, 0.000000000000000000, 0.000000000000000000 ) ) ;
#5996 = ORIENTED_EDGE ( 'NONE', *, *, #6864, .T. ) ;
#5997 = DIRECTION ( 'NONE',  ( 1.987661601597216239E-18, 4.440892098500621724E-16, 1.000000000000000000 ) ) ;
#5998 = ORIENTED_EDGE ( 'NONE', *, *, #3562, .F. ) ;
#5999 = PRODUCT_DEFINITION_SHAPE ( 'NONE', 'NONE',  #12500 ) ;
#6000 = ADVANCED_FACE ( 'NONE', ( #6834 ), #11301, .F. ) ;
#6001 = UNCERTAINTY_MEASURE_WITH_UNIT (LENGTH_MEASURE( 1.000000000000000082E-05 ), #13961, 'distance_accuracy_value', 'NONE');
#6002 = DIRECTION ( 'NONE',  ( 0.000000000000000000, 0.000000000000000000, -1.000000000000000000 ) ) ;
#6003 = CARTESIAN_POINT ( 'NONE',  ( 6.118061346828462449E-15, -30.42344490663947809, 33.00000000000002842 ) ) ;
#6004 = VECTOR ( 'NONE', #5643, 1000.000000000000000 ) ;
#6005 = ORIENTED_EDGE ( 'NONE', *, *, #6624, .T. ) ;
#6006 = CARTESIAN_POINT ( 'NONE',  ( -5.236872748402765509, -8.016972670139777574E-14, -4.357689166958463645 ) ) ;
#6007 = DIRECTION ( 'NONE',  ( 0.000000000000000000, 0.000000000000000000, 1.000000000000000000 ) ) ;
#6008 = CARTESIAN_POINT ( 'NONE',  ( 2.369999999999996998, -4.749999999999999112, -5.817072295949926440E-16 ) ) ;
#6009 = CARTESIAN_POINT ( 'NONE',  ( -28.00000000000000355, 24.50000000000001421, 8.000000000000007105 ) ) ;
#6010 = ORIENTED_EDGE ( 'NONE', *, *, #13601, .F. ) ;
#6011 = CARTESIAN_POINT ( 'NONE',  ( 21.68170757442806362, 141.2731697022877029, 28.00000000000000000 ) ) ;
#6012 = EDGE_LOOP ( 'NONE', ( #5544, #9835, #13604, #3775 ) ) ;
#6013 = CARTESIAN_POINT ( 'NONE',  ( -3.999999999999996447, -2.309401076758511806, -0.5000000000000004441 ) ) ;
#6014 = CARTESIAN_POINT ( 'NONE',  ( 0.5636734750057210697, 4.293365120987118644, -3.231543764078432357 ) ) ;
#6015 = ORIENTED_EDGE ( 'NONE', *, *, #12197, .F. ) ;
#6016 = CARTESIAN_POINT ( 'NONE',  ( 54.35294117647056567, -1.411764705882362358, 25.00000000000000000 ) ) ;
#6017 = CIRCLE ( 'NONE', #7902, 2.750000000000003553 ) ;
#6018 = DIRECTION ( 'NONE',  ( 0.000000000000000000, 0.000000000000000000, 1.000000000000000000 ) ) ;
#6019 = AXIS2_PLACEMENT_3D ( 'NONE', #9392, #12602, #2672 ) ;
#6020 = ORIENTED_EDGE ( 'NONE', *, *, #11046, .F. ) ;
#6021 = AXIS2_PLACEMENT_3D ( 'NONE', #12117, #8535, #6538 ) ;
#6022 = CARTESIAN_POINT ( 'NONE',  ( 30.07694101601105530, 130.0000000000000000, 25.00000000000000000 ) ) ;
#6023 = ORIENTED_EDGE ( 'NONE', *, *, #11542, .F. ) ;
#6024 = ADVANCED_FACE ( 'NONE', ( #3559 ), #1556, .F. ) ;
#6025 = ORIENTED_EDGE ( 'NONE', *, *, #14175, .F. ) ;
#6026 = DIRECTION ( 'NONE',  ( -1.000000000000000000, 0.000000000000000000, 0.000000000000000000 ) ) ;
#6027 = CARTESIAN_POINT ( 'NONE',  ( -3.333333333333332593, -2.694301256218264218, -3.000726591567075552 ) ) ;
#6028 = ORIENTED_EDGE ( 'NONE', *, *, #10036, .T. ) ;
#6029 = DIRECTION ( 'NONE',  ( 0.000000000000000000, 0.5000000000000012212, 0.8660254037844380415 ) ) ;
#6030 = CARTESIAN_POINT ( 'NONE',  ( 0.3572655899081733644, -2.309401076758484272, 4.000000000000031086 ) ) ;
#6031 = VERTEX_POINT ( 'NONE', #13509 ) ;
#6032 =( LENGTH_UNIT ( ) NAMED_UNIT ( * ) SI_UNIT ( .MILLI., .METRE. ) );
#6033 = CARTESIAN_POINT ( 'NONE',  ( 22.00000000000000000, 78.00000000000000000, -25.00000000000000000 ) ) ;
#6034 = VECTOR ( 'NONE', #9493, 1000.000000000000000 ) ;
#6035 = EDGE_CURVE ( 'NONE', #7658, #11064, #9271, .T. ) ;
#6036 = SURFACE_STYLE_USAGE ( .BOTH. , #2616 ) ;
#6037 = CARTESIAN_POINT ( 'NONE',  ( 20.00000000000000000, 78.00000000000000000, 25.00000000000000000 ) ) ;
#6038 = CARTESIAN_POINT ( 'NONE',  ( -4.203934431905765656, -1.640681339110420023, -3.298434044919953401 ) ) ;
#6039 = CARTESIAN_POINT ( 'NONE',  ( 5.000000000000002665, -1.947799557644007695, -0.2684016432552362441 ) ) ;
#6040 = CARTESIAN_POINT ( 'NONE',  ( 56.83050351964436686, 32.98574998546678927, -25.00000000000000000 ) ) ;
#6041 = APPLICATION_CONTEXT ( 'automotive_design' ) ;
#6042 = ORIENTED_EDGE ( 'NONE', *, *, #12325, .T. ) ;
#6043 = EDGE_CURVE ( 'NONE', #4994, #9831, #6980, .T. ) ;
#6044 = VERTEX_POINT ( 'NONE', #12397 ) ;
#6045 = VECTOR ( 'NONE', #6052, 1000.000000000000000 ) ;
#6046 = DIRECTION ( 'NONE',  ( -0.000000000000000000, -1.000000000000000000, -0.000000000000000000 ) ) ;
#6047 = ORIENTED_EDGE ( 'NONE', *, *, #5295, .T. ) ;
#6048 = DIRECTION ( 'NONE',  ( 0.2425356250363327748, -0.9701425001453319874, -0.000000000000000000 ) ) ;
#6049 = VECTOR ( 'NONE', #11030, 1000.000000000000000 ) ;
#6050 = DIRECTION ( 'NONE',  ( 0.000000000000000000, 0.000000000000000000, 1.000000000000000000 ) ) ;
#6051 = CARTESIAN_POINT ( 'NONE',  ( 118.6817075744280601, 189.5765550933606107, 33.00000000000002842 ) ) ;
#6052 = DIRECTION ( 'NONE',  ( 1.000000000000000000, 0.000000000000000000, 0.000000000000000000 ) ) ;
#6053 = DIRECTION ( 'NONE',  ( 0.000000000000000000, 0.000000000000000000, 1.000000000000000000 ) ) ;
#6054 = ORIENTED_EDGE ( 'NONE', *, *, #7451, .F. ) ;
#6055 = LINE ( 'NONE', #13630, #3542 ) ;
#6056 = CARTESIAN_POINT ( 'NONE',  ( -140.0000000000003411, 189.5765550933606107, -132.0000000000000000 ) ) ;
#6057 = CARTESIAN_POINT ( 'NONE',  ( -3.000000000000000888, 3.469446951953614189E-15, -5.974599999999997024 ) ) ;
#6058 = AXIS2_PLACEMENT_3D ( 'NONE', #11550, #11400, #5971 ) ;
#6059 = CARTESIAN_POINT ( 'NONE',  ( 20.00000000000000355, 50.00000000000000000, 25.00000000000000000 ) ) ;
#6060 = ORIENTED_EDGE ( 'NONE', *, *, #7237, .F. ) ;
#6061 = ORIENTED_EDGE ( 'NONE', *, *, #4304, .F. ) ;
#6062 = ORIENTED_EDGE ( 'NONE', *, *, #13361, .T. ) ;
#6063 = DIRECTION ( 'NONE',  ( 0.000000000000000000, 0.000000000000000000, 1.000000000000000000 ) ) ;
#6064 = CARTESIAN_POINT ( 'NONE',  ( 0.1397371499203141909, 1.362866705341260865, 3.499999999999996447 ) ) ;
#6065 =( LENGTH_UNIT ( ) NAMED_UNIT ( * ) SI_UNIT ( .MILLI., .METRE. ) );
#6066 = ORIENTED_EDGE ( 'NONE', *, *, #1647, .F. ) ;
#6067 = CARTESIAN_POINT ( 'NONE',  ( 5.211749180171794116, -2.764497899775278711, -4.327903350935043747 ) ) ;
#6068 = STYLED_ITEM ( 'NONE', ( #7212 ), #11581 ) ;
#6069 = CARTESIAN_POINT ( 'NONE',  ( 0.000000000000000000, 0.000000000000000000, 2.499999999999999112 ) ) ;
#6070 = ORIENTED_EDGE ( 'NONE', *, *, #2431, .T. ) ;
#6071 = LINE ( 'NONE', #389, #10360 ) ;
#6072 = EDGE_CURVE ( 'NONE', #13192, #10332, #10494, .T. ) ;
#6073 = EDGE_LOOP ( 'NONE', ( #10862, #5087 ) ) ;
#6074 = AXIS2_PLACEMENT_3D ( 'NONE', #1957, #5378, #1597 ) ;
#6075 = CARTESIAN_POINT ( 'NONE',  ( 22.00000000000000711, 17.00000000000000000, -25.00000000000000000 ) ) ;
#6076 = DIRECTION ( 'NONE',  ( 0.8571673007021134438, -1.049727191138620051E-16, 0.5150380749100522682 ) ) ;
#6077 = PLANE ( 'NONE',  #3903 ) ;
#6078 = ORIENTED_EDGE ( 'NONE', *, *, #3298, .T. ) ;
#6079 = VECTOR ( 'NONE', #2041, 1000.000000000000000 ) ;
#6080 = DIRECTION ( 'NONE',  ( 1.000000000000000000, -0.000000000000000000, -0.000000000000000000 ) ) ;
#6081 =( GEOMETRIC_REPRESENTATION_CONTEXT ( 3 ) GLOBAL_UNCERTAINTY_ASSIGNED_CONTEXT ( ( #13656 ) ) GLOBAL_UNIT_ASSIGNED_CONTEXT ( ( #13449, #6542, #7635 ) ) REPRESENTATION_CONTEXT ( 'NONE', 'WORKASPACE' ) );
#6082 = LINE ( 'NONE', #7109, #13045 ) ;
#6083 = ORIENTED_EDGE ( 'NONE', *, *, #10672, .T. ) ;
#6084 = CARTESIAN_POINT ( 'NONE',  ( 1.582370436563670602, 4.859920694388523366, -4.019399823475544586 ) ) ;
#6085 = CARTESIAN_POINT ( 'NONE',  ( 4.988724804725841011, 2.309401076758504701, -4.000000000000003553 ) ) ;
#6086 = VECTOR ( 'NONE', #12384, 1000.000000000000000 ) ;
#6087 = ORIENTED_EDGE ( 'NONE', *, *, #999, .F. ) ;
#6088 = FILL_AREA_STYLE ('',( #3854 ) ) ;
#6089 = ORIENTED_EDGE ( 'NONE', *, *, #2855, .F. ) ;
#6090 = CARTESIAN_POINT ( 'NONE',  ( 0.8082922630888345061, 5.306834936218050025, -0.2701150775514040703 ) ) ;
#6091 = ADVANCED_FACE ( 'NONE', ( #4852 ), #3626, .F. ) ;
#6092 = DIRECTION ( 'NONE',  ( -1.000000000000000000, 0.000000000000000000, 0.000000000000000000 ) ) ;
#6093 = ORIENTED_EDGE ( 'NONE', *, *, #2701, .T. ) ;
#6094 = DIRECTION ( 'NONE',  ( 0.000000000000000000, 0.000000000000000000, 1.000000000000000000 ) ) ;
#6095 = AXIS2_PLACEMENT_3D ( 'NONE', #217, #10388, #10534 ) ;
#6096 = CARTESIAN_POINT ( 'NONE',  ( 4.000000000000003553, -2.309401076758511806, -3.133295621305376422 ) ) ;
#6097 = COLOUR_RGB ( '', 0.31764706, 0.68627451, 0.89019608) ;
#6098 = VECTOR ( 'NONE', #4976, 1000.000000000000000 ) ;
#6099 = EDGE_CURVE ( 'NONE', #8027, #4861, #10190, .T. ) ;
#6100 = DIRECTION ( 'NONE',  ( 0.000000000000000000, 0.000000000000000000, 1.000000000000000000 ) ) ;
#6101 = ORIENTED_EDGE ( 'NONE', *, *, #10400, .T. ) ;
#6102 = ORIENTED_EDGE ( 'NONE', *, *, #1198, .T. ) ;
#6103 = DIRECTION ( 'NONE',  ( -0.000000000000000000, -1.000000000000000000, 0.000000000000000000 ) ) ;
#6104 = FACE_OUTER_BOUND ( 'NONE', #11127, .T. ) ;
#6105 = EDGE_LOOP ( 'NONE', ( #12089, #6398, #9881, #810 ) ) ;
#6106 = FACE_OUTER_BOUND ( 'NONE', #797, .T. ) ;
#6107 = FACE_OUTER_BOUND ( 'NONE', #147, .T. ) ;
#6108 = LINE ( 'NONE', #4952, #13540 ) ;
#6109 = CARTESIAN_POINT ( 'NONE',  ( 22.00000000000000355, 40.00000000000000711, 25.00000000000000000 ) ) ;
#6110 = AXIS2_PLACEMENT_3D ( 'NONE', #13336, #3312, #6655 ) ;
#6111 = ORIENTED_EDGE ( 'NONE', *, *, #10316, .F. ) ;
#6112 = DIRECTION ( 'NONE',  ( 0.000000000000000000, 8.482162385747133845E-47, -1.000000000000000000 ) ) ;
#6113 = DIRECTION ( 'NONE',  ( -0.000000000000000000, -0.000000000000000000, 1.000000000000000000 ) ) ;
#6114 = PLANE ( 'NONE',  #1587 ) ;
#6115 = ADVANCED_FACE ( 'NONE', ( #8209 ), #9163, .F. ) ;
#6116 = FACE_OUTER_BOUND ( 'NONE', #9490, .T. ) ;
#6117 = PLANE ( 'NONE',  #3469 ) ;
#6118 = VERTEX_POINT ( 'NONE', #1337 ) ;
#6119 = ADVANCED_FACE ( 'NONE', ( #5784 ), #4717, .T. ) ;
#6120 = PRESENTATION_LAYER_ASSIGNMENT (  '', '', ( #2391 ) ) ;
#6121 = ORIENTED_EDGE ( 'NONE', *, *, #14219, .F. ) ;
#6122 = VECTOR ( 'NONE', #14437, 1000.000000000000000 ) ;
#6123 = AXIS2_PLACEMENT_3D ( 'NONE', #10094, #3448, #14356 ) ;
#6124 = VERTEX_POINT ( 'NONE', #10344 ) ;
#6125 = CARTESIAN_POINT ( 'NONE',  ( 2.100000000000000977, 3.497202527569243497E-16, -4.699999999999981526 ) ) ;
#6126 = ORIENTED_EDGE ( 'NONE', *, *, #13023, .F. ) ;
#6127 = VERTEX_POINT ( 'NONE', #1935 ) ;
#6128 = FACE_OUTER_BOUND ( 'NONE', #6849, .T. ) ;
#6129 = DIRECTION ( 'NONE',  ( 0.000000000000000000, 0.000000000000000000, 1.000000000000000000 ) ) ;
#6130 = DIRECTION ( 'NONE',  ( 0.000000000000000000, 8.482162385747133845E-47, -1.000000000000000000 ) ) ;
#6131 = DIRECTION ( 'NONE',  ( 0.000000000000000000, 0.000000000000000000, -1.000000000000000000 ) ) ;
#6132 = DIRECTION ( 'NONE',  ( -0.000000000000000000, 0.000000000000000000, -1.000000000000000000 ) ) ;
#6133 = ORIENTED_EDGE ( 'NONE', *, *, #2908, .F. ) ;
#6134 = CARTESIAN_POINT ( 'NONE',  ( 0.000000000000000000, 40.49999999999999289, 0.000000000000000000 ) ) ;
#6135 =( LENGTH_UNIT ( ) NAMED_UNIT ( * ) SI_UNIT ( .MILLI., .METRE. ) );
#6136 = DIRECTION ( 'NONE',  ( -1.000000000000000000, -1.723842398015259277E-15, 0.000000000000000000 ) ) ;
#6137 = EDGE_CURVE ( 'NONE', #11237, #13192, #7685, .T. ) ;
#6138 = DIRECTION ( 'NONE',  ( 0.000000000000000000, -1.000000000000000000, 0.000000000000000000 ) ) ;
#6139 = AXIS2_PLACEMENT_3D ( 'NONE', #7558, #6250, #8449 ) ;
#6140 = EDGE_CURVE ( 'NONE', #8874, #10551, #11225, .T. ) ;
#6141 = PRODUCT_DEFINITION_SHAPE ( 'NONE', 'NONE',  #14470 ) ;
#6142 = CARTESIAN_POINT ( 'NONE',  ( 0.4317663827706312851, 5.811727376006665224, -4.566919140436428215 ) ) ;
#6143 = ORIENTED_EDGE ( 'NONE', *, *, #3370, .T. ) ;
#6144 = ORIENTED_EDGE ( 'NONE', *, *, #6681, .F. ) ;
#6145 = VERTEX_POINT ( 'NONE', #7182 ) ;
#6146 = VECTOR ( 'NONE', #13427, 1000.000000000000000 ) ;
#6147 = LINE ( 'NONE', #14214, #11993 ) ;
#6148 = CARTESIAN_POINT ( 'NONE',  ( -4.000000000000000000, -2.309401076758511806, -3.133295621305376422 ) ) ;
#6150 = CIRCLE ( 'NONE', #93, 3.000000000000001332 ) ;
#6149 = SURFACE_STYLE_FILL_AREA ( #2728 ) ;
#6151 = EDGE_CURVE ( 'NONE', #7655, #8228, #12996, .T. ) ;
#6152 = VERTEX_POINT ( 'NONE', #9542 ) ;
#6153 = EDGE_CURVE ( 'NONE', #13171, #2841, #1959, .T. ) ;
#6154 = AXIS2_PLACEMENT_3D ( 'NONE', #8851, #8256, #2715 ) ;
#6155 = FACE_OUTER_BOUND ( 'NONE', #13042, .T. ) ;
#6156 = CARTESIAN_POINT ( 'NONE',  ( 20.00000000000000355, 50.00000000000000000, -25.00000000000000000 ) ) ;
#6157 = VERTEX_POINT ( 'NONE', #11889 ) ;
#6158 = DIRECTION ( 'NONE',  ( -1.000000000000000000, -1.665334536937734071E-16, 0.000000000000000000 ) ) ;
#6159 = ADVANCED_FACE ( 'NONE', ( #11958 ), #10522, .F. ) ;
#6160 = AXIS2_PLACEMENT_3D ( 'NONE', #13457, #270, #4465 ) ;
#6161 = ORIENTED_EDGE ( 'NONE', *, *, #11383, .T. ) ;
#6162 = UNCERTAINTY_MEASURE_WITH_UNIT (LENGTH_MEASURE( 1.000000000000000082E-05 ), #5576, 'distance_accuracy_value', 'NONE');
#6163 = CARTESIAN_POINT ( 'NONE',  ( 22.00000000000000355, 40.00000000000000711, 25.00000000000000000 ) ) ;
#6164 = LINE ( 'NONE', #2817, #13011 ) ;
#6165 = DIRECTION ( 'NONE',  ( -1.000000000000000000, 0.000000000000000000, 0.000000000000000000 ) ) ;
#6166 = ORIENTED_EDGE ( 'NONE', *, *, #1624, .F. ) ;
#6167 = CARTESIAN_POINT ( 'NONE',  ( -5.236872748402764621, -0.5087250997262708907, -4.357689166958468974 ) ) ;
#6168 = DIRECTION ( 'NONE',  ( 0.000000000000000000, 0.000000000000000000, 1.000000000000000000 ) ) ;
#6169 = ORIENTED_EDGE ( 'NONE', *, *, #13019, .T. ) ;
#6170 = FACE_OUTER_BOUND ( 'NONE', #11038, .T. ) ;
#6171 = LINE ( 'NONE', #10646, #3104 ) ;
#6172 = ORIENTED_EDGE ( 'NONE', *, *, #2508, .T. ) ;
#6173 = EDGE_CURVE ( 'NONE', #5280, #8969, #14019, .T. ) ;
#6174 =( NAMED_UNIT ( * ) PLANE_ANGLE_UNIT ( ) SI_UNIT ( $, .RADIAN. ) );
#6175 = ADVANCED_FACE ( 'NONE', ( #1858 ), #6310, .F. ) ;
#6176 = CLOSED_SHELL ( 'NONE', ( #10978, #12062, #3109, #12265, #8909, #8610, #9701, #6875, #1005, #973, #7384, #2339, #659, #7125, #14415, #1403, #6908, #7606, #13524, #13823, #6942, #9994, #1059, #1633, #7836, #95, #12394, #30, #12467, #765, #4285, #520, #849, #12463, #484, #5976, #7077, #11371, #6892, #11365, #96, #8875, #2976, #5525 ) ) ;
#6177 = ORIENTED_EDGE ( 'NONE', *, *, #1612, .T. ) ;
#6178 = PLANE ( 'NONE',  #4409 ) ;
#6179 = CARTESIAN_POINT ( 'NONE',  ( 21.68170757442808849, 141.2731697022877313, 23.00000000000000000 ) ) ;
#6180 = ORIENTED_EDGE ( 'NONE', *, *, #8242, .T. ) ;
#6181 = CARTESIAN_POINT ( 'NONE',  ( 0.3461262719736172833, -4.658553426539298492, -3.371615880910392882 ) ) ;
#6182 = EDGE_CURVE ( 'NONE', #3492, #7073, #1418, .T. ) ;
#6183 = FACE_BOUND ( 'NONE', #9597, .T. ) ;
#6184 = ORIENTED_EDGE ( 'NONE', *, *, #4361, .F. ) ;
#6185 = DIRECTION ( 'NONE',  ( 1.000000000000000000, 0.000000000000000000, 0.000000000000000000 ) ) ;
#6186 = ORIENTED_EDGE ( 'NONE', *, *, #7735, .F. ) ;
#6187 = ORIENTED_EDGE ( 'NONE', *, *, #4630, .T. ) ;
#6188 = DIRECTION ( 'NONE',  ( 1.000000000000000000, 0.000000000000000000, 0.000000000000000000 ) ) ;
#6189 = EDGE_CURVE ( 'NONE', #2033, #6127, #12753, .T. ) ;
#6190 = ORIENTED_EDGE ( 'NONE', *, *, #9080, .T. ) ;
#6191 = CARTESIAN_POINT ( 'NONE',  ( 3.961551342854645608, 3.742715940867690882, -0.5174258321192194421 ) ) ;
#6192 = CARTESIAN_POINT ( 'NONE',  ( 0.000000000000000000, 0.000000000000000000, 0.000000000000000000 ) ) ;
#6193 = CARTESIAN_POINT ( 'NONE',  ( 5.000000000000000888, 0.000000000000000000, 0.000000000000000000 ) ) ;
#6194 = DIRECTION ( 'NONE',  ( -1.000000000000000000, 0.000000000000000000, 0.000000000000000000 ) ) ;
#6195 = VERTEX_POINT ( 'NONE', #10784 ) ;
#6196 = CARTESIAN_POINT ( 'NONE',  ( 22.28098402457126426, 141.4229888148238103, -28.00000000000000000 ) ) ;
#6197 = EDGE_CURVE ( 'NONE', #6262, #10783, #3989, .T. ) ;
#6198 = CARTESIAN_POINT ( 'NONE',  ( 118.6817075744280316, 109.5765550933604828, 3.299999999999976730 ) ) ;
#6199 = ADVANCED_FACE ( 'NONE', ( #8434 ), #8281, .F. ) ;
#6200 = FACE_OUTER_BOUND ( 'NONE', #4203, .T. ) ;
#6201 = CYLINDRICAL_SURFACE ( 'NONE', #12350, 3.000000000000001332 ) ;
#6202 = EDGE_CURVE ( 'NONE', #5199, #1084, #5221, .T. ) ;
#6203 = EDGE_LOOP ( 'NONE', ( #5336, #3635 ) ) ;
#6204 = CARTESIAN_POINT ( 'NONE',  ( 0.000000000000000000, -30.42444490663959300, -37.00000000000003553 ) ) ;
#6205 = VERTEX_POINT ( 'NONE', #3252 ) ;
#6206 = EDGE_CURVE ( 'NONE', #6602, #6812, #13346, .T. ) ;
#6207 = ORIENTED_EDGE ( 'NONE', *, *, #12626, .T. ) ;
#6208 = FACE_OUTER_BOUND ( 'NONE', #12925, .T. ) ;
#6209 = LINE ( 'NONE', #6051, #5580 ) ;
#6210 = CARTESIAN_POINT ( 'NONE',  ( 0.5291067203508894590, 48.48680572720346049, 0.02618951120639558677 ) ) ;
#6211 = DIRECTION ( 'NONE',  ( -1.000000000000000000, 0.000000000000000000, 0.000000000000000000 ) ) ;
#6212 = EDGE_LOOP ( 'NONE', ( #10073, #9171 ) ) ;
#6213 = FACE_OUTER_BOUND ( 'NONE', #5159, .T. ) ;
#6214 = DIRECTION ( 'NONE',  ( 0.000000000000000000, 0.000000000000000000, 1.000000000000000000 ) ) ;
#6215 = CARTESIAN_POINT ( 'NONE',  ( 4.055492966679429045, -3.795017426214134293, 0.5629142681437507845 ) ) ;
#6216 = ORIENTED_EDGE ( 'NONE', *, *, #6072, .F. ) ;
#6217 = CARTESIAN_POINT ( 'NONE',  ( -3.074732204440936414E-15, -3.070647092368440134, -2.681483223904212121 ) ) ;
#6218 = ORIENTED_EDGE ( 'NONE', *, *, #3876, .F. ) ;
#6219 = ORIENTED_EDGE ( 'NONE', *, *, #9461, .F. ) ;
#6220 = EDGE_CURVE ( 'NONE', #9772, #3097, #13275, .T. ) ;
#6221 = FACE_OUTER_BOUND ( 'NONE', #4366, .T. ) ;
#6222 = CARTESIAN_POINT ( 'NONE',  ( 0.000000000000000000, 48.49999999999999289, 8.000000000000007105 ) ) ;
#6223 = SURFACE_SIDE_STYLE ('',( #6149 ) ) ;
#6224 = ORIENTED_EDGE ( 'NONE', *, *, #756, .T. ) ;
#6225 = CARTESIAN_POINT ( 'NONE',  ( 1.721886139900713042, -5.052888355618668115, -4.357689166958440552 ) ) ;
#6226 = DIRECTION ( 'NONE',  ( 0.000000000000000000, 0.000000000000000000, 1.000000000000000000 ) ) ;
#6227 = CIRCLE ( 'NONE', #3671, 5.499999999999980460 ) ;
#6228 = ORIENTED_EDGE ( 'NONE', *, *, #12813, .T. ) ;
#6229 = CARTESIAN_POINT ( 'NONE',  ( 20.00000000000000711, 20.00000000000000355, -25.00000000000000000 ) ) ;
#6230 = EDGE_CURVE ( 'NONE', #6341, #8772, #7546, .T. ) ;
#6231 = VECTOR ( 'NONE', #1186, 1000.000000000000000 ) ;
#6232 = ADVANCED_FACE ( 'NONE', ( #13141 ), #5359, .T. ) ;
#6233 = DIRECTION ( 'NONE',  ( -1.000000000000000000, -1.723842398015259277E-15, 0.000000000000000000 ) ) ;
#6234 = CARTESIAN_POINT ( 'NONE',  ( 1.560000000000005826, 1.732050807568871864, 0.000000000000000000 ) ) ;
#6235 = DIRECTION ( 'NONE',  ( 2.273843122241288438E-18, 5.551115123125783935E-17, 1.000000000000000000 ) ) ;
#6236 = ORIENTED_EDGE ( 'NONE', *, *, #13087, .T. ) ;
#6237 = CARTESIAN_POINT ( 'NONE',  ( 3.370256023960729782E-15, 5.773502691896274186, -4.284345921091780696 ) ) ;
#6238 = CARTESIAN_POINT ( 'NONE',  ( 0.000000000000000000, 4.618802153517016507, -3.133295621305376422 ) ) ;
#6239 = VERTEX_POINT ( 'NONE', #7690 ) ;
#6240 = CARTESIAN_POINT ( 'NONE',  ( 4.942464816487918355, 4.274687029205021638, -0.5960248789591272578 ) ) ;
#6241 = DIRECTION ( 'NONE',  ( 0.000000000000000000, 0.000000000000000000, -1.000000000000000000 ) ) ;
#6242 = VECTOR ( 'NONE', #3205, 1000.000000000000000 ) ;
#6243 = VERTEX_POINT ( 'NONE', #1048 ) ;
#6244 = LINE ( 'NONE', #13338, #4942 ) ;
#6245 = ORIENTED_EDGE ( 'NONE', *, *, #9223, .F. ) ;
#6246 = LINE ( 'NONE', #8521, #5083 ) ;
#6247 = PLANE ( 'NONE',  #7755 ) ;
#6248 = VERTEX_POINT ( 'NONE', #14444 ) ;
#6249 = DIRECTION ( 'NONE',  ( 1.000000000000000000, 0.000000000000000000, -0.000000000000000000 ) ) ;
#6250 = DIRECTION ( 'NONE',  ( -0.9701425001453319874, -0.2425356250363330801, 0.000000000000000000 ) ) ;
#6251 = AXIS2_PLACEMENT_3D ( 'NONE', #10117, #9077, #5925 ) ;
#6252 = ORIENTED_EDGE ( 'NONE', *, *, #11582, .T. ) ;
#6253 = AXIS2_PLACEMENT_3D ( 'NONE', #8606, #5097, #9498 ) ;
#6254 = CYLINDRICAL_SURFACE ( 'NONE', #331, 3.000000000000000888 ) ;
#6255 = CARTESIAN_POINT ( 'NONE',  ( -2.176667689905601222, -4.790324513057892197, -4.357749648769125628 ) ) ;
#6256 = ORIENTED_EDGE ( 'NONE', *, *, #9790, .T. ) ;
#6257 = CARTESIAN_POINT ( 'NONE',  ( 3.950241966888154099, 3.393956070637165201, -1.121495646999262075 ) ) ;
#6258 = PRODUCT_DEFINITION_SHAPE ( 'NONE', 'NONE',  #14485 ) ;
#6259 = CYLINDRICAL_SURFACE ( 'NONE', #5987, 2.500000000000002220 ) ;
#6260 = FILL_AREA_STYLE_COLOUR ( '', #5780 ) ;
#6261 = DIRECTION ( 'NONE',  ( -0.000000000000000000, -1.000000000000000000, -0.000000000000000000 ) ) ;
#6262 = VERTEX_POINT ( 'NONE', #12033 ) ;
#6263 = VECTOR ( 'NONE', #1548, 1000.000000000000000 ) ;
#6264 = LINE ( 'NONE', #9713, #12799 ) ;
#6265 = CIRCLE ( 'NONE', #13532, 2.500000000000002220 ) ;
#6266 = CARTESIAN_POINT ( 'NONE',  ( 0.000000000000000000, 4.618802153517016507, -0.5000000000000004441 ) ) ;
#6267 = CIRCLE ( 'NONE', #1351, 2.500000000000002220 ) ;
#6268 = ADVANCED_BREP_SHAPE_REPRESENTATION ( '', ( #11686, #11025 ), #12660 ) ;
#6269 = EDGE_LOOP ( 'NONE', ( #209, #2008, #4493, #3783 ) ) ;
#6270 = EDGE_CURVE ( 'NONE', #172, #14160, #2653, .T. ) ;
#6271 = CARTESIAN_POINT ( 'NONE',  ( 28.00000000000000355, 29.99999999999999645, -24.99999999999999289 ) ) ;
#6272 = ORIENTED_EDGE ( 'NONE', *, *, #8315, .F. ) ;
#6273 = EDGE_CURVE ( 'NONE', #2047, #10405, #9827, .T. ) ;
#6274 = ORIENTED_EDGE ( 'NONE', *, *, #8411, .T. ) ;
#6275 = PRESENTATION_LAYER_ASSIGNMENT (  '', '', ( #14006 ) ) ;
#6276 = CARTESIAN_POINT ( 'NONE',  ( 49.40514726928103073, 42.68717498692012668, -25.00000000000000000 ) ) ;
#6277 = DIRECTION ( 'NONE',  ( 0.000000000000000000, 0.000000000000000000, -1.000000000000000000 ) ) ;
#6278 = FACE_OUTER_BOUND ( 'NONE', #13428, .T. ) ;
#6279 = DIRECTION ( 'NONE',  ( 0.000000000000000000, 0.000000000000000000, 1.000000000000000000 ) ) ;
#6280 = LINE ( 'NONE', #9725, #3318 ) ;
#6281 = PRODUCT_CONTEXT ( 'NONE', #5833, 'mechanical' ) ;
#6282 = CARTESIAN_POINT ( 'NONE',  ( 0.000000000000000000, 4.862606272033096033, -3.445885042887453231 ) ) ;
#6283 = DIRECTION ( 'NONE',  ( 0.000000000000000000, 0.000000000000000000, -1.000000000000000000 ) ) ;
#6284 = ORIENTED_EDGE ( 'NONE', *, *, #5175, .T. ) ;
#6285 = ADVANCED_FACE ( 'NONE', ( #892, #5571 ), #12167, .T. ) ;
#6286 = CARTESIAN_POINT ( 'NONE',  ( 5.253368672218638125, 3.033033817057769532, -4.659491423763650886 ) ) ;
#6287 = ORIENTED_EDGE ( 'NONE', *, *, #13778, .T. ) ;
#6288 = VECTOR ( 'NONE', #3883, 1000.000000000000000 ) ;
#6289 = ADVANCED_FACE ( 'NONE', ( #4505 ), #14281, .F. ) ;
#6290 = ORIENTED_EDGE ( 'NONE', *, *, #2515, .F. ) ;
#6291 = VERTEX_POINT ( 'NONE', #6517 ) ;
#6292 = CARTESIAN_POINT ( 'NONE',  ( 105.6817075744280174, 69.57655509336051125, 1.592040838891559450E-14 ) ) ;
#6293 = FACE_OUTER_BOUND ( 'NONE', #6456, .T. ) ;
#6294 = CIRCLE ( 'NONE', #11666, 5.499999999999980460 ) ;
#6295 =( LENGTH_UNIT ( ) NAMED_UNIT ( * ) SI_UNIT ( .MILLI., .METRE. ) );
#6296 = EDGE_LOOP ( 'NONE', ( #11156, #5741, #6787, #5765 ) ) ;
#6297 = CARTESIAN_POINT ( 'NONE',  ( 20.00000000000000000, 37.00000000000000711, -25.00000000000000000 ) ) ;
#6298 = EDGE_CURVE ( 'NONE', #10870, #2316, #4437, .T. ) ;
#6299 = CARTESIAN_POINT ( 'NONE',  ( 64.03192852109765454, -5.819950020346492892, 25.00000000000000000 ) ) ;
#6300 = VERTEX_POINT ( 'NONE', #4292 ) ;
#6301 = CARTESIAN_POINT ( 'NONE',  ( 27.75000000000001066, 0.000000000000000000, 0.000000000000000000 ) ) ;
#6302 = ORIENTED_EDGE ( 'NONE', *, *, #10686, .F. ) ;
#6303 = VECTOR ( 'NONE', #9721, 1000.000000000000000 ) ;
#6304 = VERTEX_POINT ( 'NONE', #13353 ) ;
#6305 = UNCERTAINTY_MEASURE_WITH_UNIT (LENGTH_MEASURE( 1.000000000000000082E-05 ), #10838, 'distance_accuracy_value', 'NONE');
#6306 = LINE ( 'NONE', #14297, #4699 ) ;
#6307 = CYLINDRICAL_SURFACE ( 'NONE', #11116, 5.000000000000018652 ) ;
#6308 = CARTESIAN_POINT ( 'NONE',  ( 18.68170757442808849, 141.2731697022877313, -35.00000000000000000 ) ) ;
#6309 = ORIENTED_EDGE ( 'NONE', *, *, #3965, .F. ) ;
#6310 = CYLINDRICAL_SURFACE ( 'NONE', #11450, 3.299999999999976730 ) ;
#6311 = CARTESIAN_POINT ( 'NONE',  ( 20.00000000000000000, 60.00000000000000711, -25.00000000000000000 ) ) ;
#6312 = SURFACE_STYLE_FILL_AREA ( #6599 ) ;
#6313 = EDGE_LOOP ( 'NONE', ( #12345, #744, #4408, #12438 ) ) ;
#6314 = ORIENTED_EDGE ( 'NONE', *, *, #6633, .F. ) ;
#6315 = CONICAL_SURFACE ( 'NONE', #14, 5.000000000000000888, 0.9110539511682884672 ) ;
#6316 = DIRECTION ( 'NONE',  ( -1.000000000000000000, 0.000000000000000000, 0.000000000000000000 ) ) ;
#6317 = VECTOR ( 'NONE', #2922, 1000.000000000000000 ) ;
#6318 = EDGE_LOOP ( 'NONE', ( #4827, #10368, #7775, #13080, #3875 ) ) ;
#6319 = DIRECTION ( 'NONE',  ( -0.000000000000000000, 0.000000000000000000, 1.000000000000000000 ) ) ;
#6320 = EDGE_CURVE ( 'NONE', #5614, #10014, #14231, .T. ) ;
#6321 = ADVANCED_FACE ( 'NONE', ( #9821 ), #11426, .T. ) ;
#6322 = CARTESIAN_POINT ( 'NONE',  ( -0.1750032273043237441, -4.719840313910227181, -3.169254239516205107 ) ) ;
#6323 = ORIENTED_EDGE ( 'NONE', *, *, #7480, .F. ) ;
#6324 = PLANE ( 'NONE',  #10205 ) ;
#6325 = CARTESIAN_POINT ( 'NONE',  ( 40.00000000000000711, 80.00000000000000000, 25.00000000000000000 ) ) ;
#6326 = ORIENTED_EDGE ( 'NONE', *, *, #14383, .F. ) ;
#6327 = CIRCLE ( 'NONE', #7260, 2.100000000000000977 ) ;
#6328 = EDGE_LOOP ( 'NONE', ( #11727, #13455, #12853, #9143 ) ) ;
#6329 = CARTESIAN_POINT ( 'NONE',  ( -2.750000000000003997, 40.49999999999999289, 8.000000000000007105 ) ) ;
#6330 = CARTESIAN_POINT ( 'NONE',  ( 20.00000000000000355, 17.00000000000000000, -25.00000000000000000 ) ) ;
#6331 = ORIENTED_EDGE ( 'NONE', *, *, #3621, .F. ) ;
#6332 = AXIS2_PLACEMENT_3D ( 'NONE', #14091, #9818, #8723 ) ;
#6333 = CARTESIAN_POINT ( 'NONE',  ( 4.170895651974873886, -4.109780709045213420, -7.786222839923386950E-14 ) ) ;
#6334 = LINE ( 'NONE', #6405, #5563 ) ;
#6335 =( NAMED_UNIT ( * ) SI_UNIT ( $, .STERADIAN. ) SOLID_ANGLE_UNIT ( ) );
#6336 = DIRECTION ( 'NONE',  ( 1.000000000000000000, 0.000000000000000000, 0.000000000000000000 ) ) ;
#6337 = ORIENTED_EDGE ( 'NONE', *, *, #6678, .F. ) ;
#6338 = CARTESIAN_POINT ( 'NONE',  ( 20.00000000000000000, 37.00000000000000711, 25.00000000000000000 ) ) ;
#6339 = VECTOR ( 'NONE', #8037, 1000.000000000000000 ) ;
#6340 = VECTOR ( 'NONE', #1906, 1000.000000000000000 ) ;
#6341 = VERTEX_POINT ( 'NONE', #11207 ) ;
#6342 = ORIENTED_EDGE ( 'NONE', *, *, #9212, .T. ) ;
#6343 = LINE ( 'NONE', #7726, #13187 ) ;
#6344 = VERTEX_POINT ( 'NONE', #7773 ) ;
#6345 = VERTEX_POINT ( 'NONE', #10916 ) ;
#6346 = CARTESIAN_POINT ( 'NONE',  ( -6.938893903907228378E-15, 24.50000000000002132, 8.000000000000007105 ) ) ;
#6347 = CIRCLE ( 'NONE', #12195, 5.000000000000004441 ) ;
#6348 = CIRCLE ( 'NONE', #4955, 2.749999999999997780 ) ;
#6349 = CARTESIAN_POINT ( 'NONE',  ( 20.00000000000000000, 80.00000000000000000, 25.00000000000000000 ) ) ;
#6350 = CARTESIAN_POINT ( 'NONE',  ( 0.2655919857739733603, 48.49999999999999289, 9.644881826068967185E-16 ) ) ;
#6351 = FACE_OUTER_BOUND ( 'NONE', #3913, .T. ) ;
#6352 = DIRECTION ( 'NONE',  ( 0.000000000000000000, 1.000000000000000000, 0.000000000000000000 ) ) ;
#6353 = SHAPE_DEFINITION_REPRESENTATION ( #13869, #1400 ) ;
#6354 = CARTESIAN_POINT ( 'NONE',  ( 3.861362476283259237, 2.629030857715991321, -3.371615880910392882 ) ) ;
#6355 = CARTESIAN_POINT ( 'NONE',  ( 28.00000000000000355, 29.99999999999999645, -34.50000000000000000 ) ) ;
#6356 = EDGE_CURVE ( 'NONE', #1, #7928, #1115, .T. ) ;
#6357 = ADVANCED_FACE ( 'NONE', ( #8938 ), #13434, .T. ) ;
#6358 = VERTEX_POINT ( 'NONE', #13208 ) ;
#6359 =( GEOMETRIC_REPRESENTATION_CONTEXT ( 3 ) GLOBAL_UNCERTAINTY_ASSIGNED_CONTEXT ( ( #6162 ) ) GLOBAL_UNIT_ASSIGNED_CONTEXT ( ( #5576, #9011, #5707 ) ) REPRESENTATION_CONTEXT ( 'NONE', 'WORKASPACE' ) );
#6360 = AXIS2_PLACEMENT_3D ( 'NONE', #3396, #8717, #8855 ) ;
#6361 = DIRECTION ( 'NONE',  ( -0.000000000000000000, -0.000000000000000000, 1.000000000000000000 ) ) ;
#6362 = EDGE_LOOP ( 'NONE', ( #2102, #14111, #9532, #8530 ) ) ;
#6363 = EDGE_CURVE ( 'NONE', #14451, #3625, #4358, .T. ) ;
#6364 = CARTESIAN_POINT ( 'NONE',  ( 5.551115123125782702E-14, 1.387778780781445676E-14, -4.000000000000003553 ) ) ;
#6365 = ORIENTED_EDGE ( 'NONE', *, *, #12875, .T. ) ;
#6366 = CARTESIAN_POINT ( 'NONE',  ( 32.50229726637438432, 120.2985749985466839, -25.00000000000000000 ) ) ;
#6367 = CARTESIAN_POINT ( 'NONE',  ( 5.000000000000000888, 0.2466074518009269412, -6.594151494374726167E-16 ) ) ;
#6368 = EDGE_CURVE ( 'NONE', #2567, #5483, #514, .T. ) ;
#6369 =( GEOMETRIC_REPRESENTATION_CONTEXT ( 3 ) GLOBAL_UNCERTAINTY_ASSIGNED_CONTEXT ( ( #10848 ) ) GLOBAL_UNIT_ASSIGNED_CONTEXT ( ( #11208, #1392, #1262 ) ) REPRESENTATION_CONTEXT ( 'NONE', 'WORKASPACE' ) );
#6370 = AXIS2_PLACEMENT_3D ( 'NONE', #1233, #3705, #6018 ) ;
#6371 = VECTOR ( 'NONE', #10969, 1000.000000000000114 ) ;
#6372 = ORIENTED_EDGE ( 'NONE', *, *, #13541, .F. ) ;
#6373 = EDGE_CURVE ( 'NONE', #7928, #12216, #14254, .T. ) ;
#6374 = VERTEX_POINT ( 'NONE', #5045 ) ;
#6375 = DIRECTION ( 'NONE',  ( -1.000000000000000000, 0.000000000000000000, 0.000000000000000000 ) ) ;
#6376 = CARTESIAN_POINT ( 'NONE',  ( -4.400655246570308599, -3.515428273945673698, -4.476900509771408743 ) ) ;
#6377 = B_SPLINE_CURVE_WITH_KNOTS ( 'NONE', 3,
 ( #10398, #1318, #11347, #379, #9072 ),
 .UNSPECIFIED., .F., .F.,
 ( 4, 1, 4 ),
 ( 0.000000000000000000, 0.002309401076758504923, 0.004618802153517009845 ),
 .UNSPECIFIED. ) ;
#6378 = CARTESIAN_POINT ( 'NONE',  ( 20.00000000000000000, -5.510910596163090344E-15, 25.00000000000000000 ) ) ;
#6379 = CIRCLE ( 'NONE', #5668, 4.999999999999988454 ) ;
#6380 = DIRECTION ( 'NONE',  ( -1.000000000000000000, -1.913084959030911013E-15, -0.000000000000000000 ) ) ;
#6381 = DIRECTION ( 'NONE',  ( 1.000000000000000000, 0.000000000000000000, 0.000000000000000000 ) ) ;
#6382 = CARTESIAN_POINT ( 'NONE',  ( 71.80728622811317052, 38.49793223363091954, -28.00000000000000000 ) ) ;
#6383 = ORIENTED_EDGE ( 'NONE', *, *, #8329, .F. ) ;
#6384 = EDGE_CURVE ( 'NONE', #8545, #2739, #8176, .T. ) ;
#6385 = CARTESIAN_POINT ( 'NONE',  ( 4.170895651974874774, 4.109780709045202762, 1.691345105195479668E-14 ) ) ;
#6386 = DIRECTION ( 'NONE',  ( 0.000000000000000000, 0.000000000000000000, -1.000000000000000000 ) ) ;
#6387 = AXIS2_PLACEMENT_3D ( 'NONE', #11192, #218, #7754 ) ;
#6388 = CARTESIAN_POINT ( 'NONE',  ( 1.734723475976807094E-14, 35.49999999999996447, 8.000000000000007105 ) ) ;
#6389 = ORIENTED_EDGE ( 'NONE', *, *, #12539, .F. ) ;
#6390 = ORIENTED_EDGE ( 'NONE', *, *, #10673, .T. ) ;
#6391 = DIRECTION ( 'NONE',  ( 0.000000000000000000, 1.000000000000000000, 0.000000000000000000 ) ) ;
#6392 = DIRECTION ( 'NONE',  ( 0.000000000000000000, 0.000000000000000000, 1.000000000000000000 ) ) ;
#6393 = TOROIDAL_SURFACE ( 'NONE', #3391, 5.200000000000001066, 0.4999999999999975020 ) ;
#6394 = ORIENTED_EDGE ( 'NONE', *, *, #3988, .T. ) ;
#6395 = CARTESIAN_POINT ( 'NONE',  ( 30.60000000000001563, 0.000000000000000000, 0.000000000000000000 ) ) ;
#6396 = CARTESIAN_POINT ( 'NONE',  ( 5.185163620695915299, -2.993655612202863470, -4.630826434870603414 ) ) ;
#6397 = VERTEX_POINT ( 'NONE', #9510 ) ;
#6398 = ORIENTED_EDGE ( 'NONE', *, *, #8142, .F. ) ;
#6399 = DIRECTION ( 'NONE',  ( -1.000000000000000000, 0.000000000000000000, 0.000000000000000000 ) ) ;
#6400 = CARTESIAN_POINT ( 'NONE',  ( 0.000000000000000000, 48.49999999999999289, 0.000000000000000000 ) ) ;
#6401 = ADVANCED_FACE ( 'NONE', ( #6817 ), #11697, .T. ) ;
#6402 = ORIENTED_EDGE ( 'NONE', *, *, #6099, .F. ) ;
#6403 = DIRECTION ( 'NONE',  ( 0.000000000000000000, 0.000000000000000000, -1.000000000000000000 ) ) ;
#6404 = LINE ( 'NONE', #7144, #7251 ) ;
#6405 = CARTESIAN_POINT ( 'NONE',  ( 6.800000000000028244, 2.309401076758498039, 4.000000000000003553 ) ) ;
#6406 = DIRECTION ( 'NONE',  ( 0.000000000000000000, 0.5000000000000011102, -0.8660254037844379305 ) ) ;
#6407 = ORIENTED_EDGE ( 'NONE', *, *, #12964, .T. ) ;
#6408 = SURFACE_SIDE_STYLE ('',( #11606 ) ) ;
#6409 = ORIENTED_EDGE ( 'NONE', *, *, #8756, .F. ) ;
#6410 = DIRECTION ( 'NONE',  ( 1.000000000000000000, 0.000000000000000000, 0.000000000000000000 ) ) ;
#6411 = CARTESIAN_POINT ( 'NONE',  ( 32.50229726637438432, 120.2985749985466839, 25.00000000000000000 ) ) ;
#6412 = EDGE_LOOP ( 'NONE', ( #13282, #5461, #11058, #4784 ) ) ;
#6413 = CARTESIAN_POINT ( 'NONE',  ( 24.99999999999999289, -4.898587196589414604E-15, -25.00000000000000000 ) ) ;
#6414 = ADVANCED_FACE ( 'NONE', ( #8399 ), #10179, .F. ) ;
#6415 = ORIENTED_EDGE ( 'NONE', *, *, #3513, .T. ) ;
#6416 = CARTESIAN_POINT ( 'NONE',  ( 20.00000000000000000, 80.00000000000000000, -25.00000000000000000 ) ) ;
#6417 = EDGE_CURVE ( 'NONE', #13711, #2554, #13098, .T. ) ;
#6418 = CARTESIAN_POINT ( 'NONE',  ( 49.47979101891770171, 52.38859998837343568, 25.00000000000000000 ) ) ;
#6419 = CARTESIAN_POINT ( 'NONE',  ( 0.000000000000000000, 40.49999999999999289, 8.000000000000007105 ) ) ;
#6420 = FACE_OUTER_BOUND ( 'NONE', #189, .T. ) ;
#6421 = DIRECTION ( 'NONE',  ( 0.000000000000000000, 0.000000000000000000, 1.000000000000000000 ) ) ;
#6422 = APPLICATION_PROTOCOL_DEFINITION ( 'draft international standard', 'automotive_design', 1998, #14381 ) ;
#6423 = DIRECTION ( 'NONE',  ( 1.000000000000000000, 0.000000000000000000, 0.000000000000000000 ) ) ;
#6424 = CARTESIAN_POINT ( 'NONE',  ( 34.85300976710104948, 100.8957249956400375, -25.00000000000000000 ) ) ;
#6425 = ORIENTED_EDGE ( 'NONE', *, *, #5849, .T. ) ;
#6426 = CARTESIAN_POINT ( 'NONE',  ( 4.071447262713911996, -2.020725942163681399, 3.499999999999989342 ) ) ;
#6427 = CARTESIAN_POINT ( 'NONE',  ( 62.10586122665984732, -20.42344490663941414, 35.00000000000000000 ) ) ;
#6428 = EDGE_LOOP ( 'NONE', ( #11229, #10714 ) ) ;
#6429 = DIRECTION ( 'NONE',  ( 0.000000000000000000, 0.000000000000000000, 1.000000000000000000 ) ) ;
#6430 = CARTESIAN_POINT ( 'NONE',  ( 5.000000000000002665, 0.4965892259340556336, -0.01450341304856543785 ) ) ;
#6431 = LINE ( 'NONE', #12081, #8667 ) ;
#6432 = ORIENTED_EDGE ( 'NONE', *, *, #2623, .T. ) ;
#6433 = DIRECTION ( 'NONE',  ( 0.000000000000000000, 0.000000000000000000, -1.000000000000000000 ) ) ;
#6434 = LINE ( 'NONE', #6156, #10557 ) ;
#6435 = ADVANCED_FACE ( 'NONE', ( #3814 ), #7146, .F. ) ;
#6436 = LINE ( 'NONE', #8644, #3376 ) ;
#6437 = CARTESIAN_POINT ( 'NONE',  ( -3.540000644887378645, -2.810673041921230020, -3.302142222889056455 ) ) ;
#6438 = PRODUCT_DEFINITION_CONTEXT ( 'detailed design', #645, 'design' ) ;
#6439 = EDGE_CURVE ( 'NONE', #5531, #8011, #9354, .T. ) ;
#6440 = LINE ( 'NONE', #3177, #2593 ) ;
#6441 = CARTESIAN_POINT ( 'NONE',  ( 20.00000000000000000, 37.00000000000000711, 25.00000000000000000 ) ) ;
#6442 = FACE_OUTER_BOUND ( 'NONE', #12476, .T. ) ;
#6443 = EDGE_CURVE ( 'NONE', #9934, #5064, #5639, .T. ) ;
#6444 = CARTESIAN_POINT ( 'NONE',  ( 3.972709601346603225, -2.746729940827184802, 2.374099244652728924 ) ) ;
#6445 = CARTESIAN_POINT ( 'NONE',  ( -31.96535124910143821, 127.8614049964057813, 1.219362754841566419E-12 ) ) ;
#6446 = CARTESIAN_POINT ( 'NONE',  ( 22.00000000000000000, 60.00000000000000711, 25.00000000000000000 ) ) ;
#6447 = EDGE_LOOP ( 'NONE', ( #13595, #14022 ) ) ;
#6448 = AXIS2_PLACEMENT_3D ( 'NONE', #3986, #8431, #7400 ) ;
#6449 = ORIENTED_EDGE ( 'NONE', *, *, #3027, .T. ) ;
#6450 = DIRECTION ( 'NONE',  ( 0.8660254037844378194, -0.5000000000000014433, 0.000000000000000000 ) ) ;
#6451 = CARTESIAN_POINT ( 'NONE',  ( 1.360615521534842998, -4.061278559077564410, -3.205052026701877388 ) ) ;
#6452 = ORIENTED_EDGE ( 'NONE', *, *, #12896, .T. ) ;
#6453 = CARTESIAN_POINT ( 'NONE',  ( 118.6817075744280601, 189.5765550933606107, -117.0000000000000000 ) ) ;
#6454 = ADVANCED_FACE ( 'NONE', ( #10112 ), #9004, .F. ) ;
#6455 = DIRECTION ( 'NONE',  ( 1.000000000000000000, 1.665334536937734071E-16, 0.000000000000000000 ) ) ;
#6456 = EDGE_LOOP ( 'NONE', ( #8538, #12170, #13518, #11251 ) ) ;
#6457 = ORIENTED_EDGE ( 'NONE', *, *, #12716, .F. ) ;
#6458 = FACE_OUTER_BOUND ( 'NONE', #1022, .T. ) ;
#6459 = CARTESIAN_POINT ( 'NONE',  ( 18.68170757442808849, 141.2731697022877313, 23.00000000000000000 ) ) ;
#6460 = ORIENTED_EDGE ( 'NONE', *, *, #1546, .T. ) ;
#6461 = VECTOR ( 'NONE', #12041, 1000.000000000000000 ) ;
#6462 = CARTESIAN_POINT ( 'NONE',  ( 4.052424581288006422, -3.786734753435994083, -0.5771415817964102857 ) ) ;
#6463 = DIRECTION ( 'NONE',  ( 0.000000000000000000, 8.482162385747133845E-47, -1.000000000000000000 ) ) ;
#6464 = VECTOR ( 'NONE', #12491, 999.9999999999998863 ) ;
#6465 = PLANE ( 'NONE',  #14233 ) ;
#6466 = B_SPLINE_CURVE_WITH_KNOTS ( 'NONE', 3,
 ( #8551, #6482, #5188, #9789, #10889, #8483, #11783, #667, #14339, #9723, #14267, #859, #13032, #8694, #11926, #3152, #10958, #7582, #927, #14198, #9655, #8623, #11852, #4180, #3216, #3013, #8762, #7443, #13241, #2941, #1757, #6210, #6350, #10680 ),
 .UNSPECIFIED., .F., .F.,
 ( 4, 2, 2, 2, 2, 2, 2, 2, 2, 2, 2, 2, 2, 2, 2, 2, 4 ),
 ( 0.000000000000000000, 0.0007952457144059375989, 0.001590491428811875198, 0.002385737143217811929, 0.003180982857623748661, 0.003976228572029685826, 0.004771474286435622991, 0.005566720000841560156, 0.006361965715247496454, 0.007157211429653435354, 0.007952457144059375121, 0.008747702858465312287, 0.009542948572871252921, 0.01033819428727719182, 0.01113344000168312899, 0.01192868571608906962, 0.01272393143049500679 ),
 .UNSPECIFIED. ) ;
#6467 = CARTESIAN_POINT ( 'NONE',  ( -5.284804376168110274, 3.015249596956810940, -4.666192694417969022 ) ) ;
#6468 = ORIENTED_EDGE ( 'NONE', *, *, #9520, .T. ) ;
#6469 = CARTESIAN_POINT ( 'NONE',  ( 49.55443476855437268, 62.09002498982675888, -25.00000000000000000 ) ) ;
#6470 = CARTESIAN_POINT ( 'NONE',  ( 28.00000000000000355, 29.99999999999999645, -34.50000000000000000 ) ) ;
#6471 = AXIS2_PLACEMENT_3D ( 'NONE', #478, #1797, #12929 ) ;
#6472 = EDGE_CURVE ( 'NONE', #3067, #45, #8253, .T. ) ;
#6473 = CIRCLE ( 'NONE', #2512, 5.371010071662830399 ) ;
#6474 = ORIENTED_EDGE ( 'NONE', *, *, #12008, .T. ) ;
#6475 = ORIENTED_EDGE ( 'NONE', *, *, #8362, .F. ) ;
#6476 = ORIENTED_EDGE ( 'NONE', *, *, #2084, .F. ) ;
#6477 = DIRECTION ( 'NONE',  ( 0.9701425001453319874, 0.2425356250363328026, 0.000000000000000000 ) ) ;
#6478 = ORIENTED_EDGE ( 'NONE', *, *, #13008, .T. ) ;
#6479 = LINE ( 'NONE', #7580, #1880 ) ;
#6480 = CARTESIAN_POINT ( 'NONE',  ( 5.244818697407748864, -2.029379090245567063, -4.490884354499014464 ) ) ;
#6481 = AXIS2_PLACEMENT_3D ( 'NONE', #14082, #3977, #4061 ) ;
#6482 = CARTESIAN_POINT ( 'NONE',  ( 0.2691907178497377484, 48.49999999999999289, 8.000000000000008882 ) ) ;
#6483 = DIRECTION ( 'NONE',  ( 0.000000000000000000, 1.000000000000000000, -0.000000000000000000 ) ) ;
#6484 = AXIS2_PLACEMENT_3D ( 'NONE', #3696, #1720, #4931 ) ;
#6485 = CARTESIAN_POINT ( 'NONE',  ( 71.80728622811317052, -17.99808865627607801, 28.00000000000000000 ) ) ;
#6486 = APPLICATION_PROTOCOL_DEFINITION ( 'draft international standard', 'automotive_design', 1998, #8847 ) ;
#6487 = AXIS2_PLACEMENT_3D ( 'NONE', #13798, #7185, #2516 ) ;
#6488 = CARTESIAN_POINT ( 'NONE',  ( -5.000000000000000888, 0.000000000000000000, 0.000000000000000000 ) ) ;
#6489 = FACE_OUTER_BOUND ( 'NONE', #838, .T. ) ;
#6490 = PRODUCT_DEFINITION_SHAPE ( 'NONE', 'NONE',  #14489 ) ;
#6491 = ORIENTED_EDGE ( 'NONE', *, *, #12525, .F. ) ;
#6492 = AXIS2_PLACEMENT_3D ( 'NONE', #9314, #249, #2514 ) ;
#6493 = EDGE_CURVE ( 'NONE', #5199, #2483, #3467, .T. ) ;
#6494 = EDGE_CURVE ( 'NONE', #13612, #6124, #1530, .T. ) ;
#6495 = CARTESIAN_POINT ( 'NONE',  ( 4.851472949721050476, 2.694301256218257112, 3.333333333333363679 ) ) ;
#6496 = ORIENTED_EDGE ( 'NONE', *, *, #1938, .T. ) ;
#6497 = CIRCLE ( 'NONE', #4642, 2.600000000000004974 ) ;
#6498 = CARTESIAN_POINT ( 'NONE',  ( 108.6817075744280459, 109.5765550933604828, 0.000000000000000000 ) ) ;
#6499 = VECTOR ( 'NONE', #12553, 1000.000000000000000 ) ;
#6500 = CARTESIAN_POINT ( 'NONE',  ( 0.000000000000000000, 0.000000000000000000, 1.599999999999990319 ) ) ;
#6501 = LINE ( 'NONE', #9886, #11235 ) ;
#6502 = CARTESIAN_POINT ( 'NONE',  ( 4.862831555538840611, 4.276542471545668356, -0.5928111585567288344 ) ) ;
#6503 = FACE_OUTER_BOUND ( 'NONE', #12259, .T. ) ;
#6504 =( NAMED_UNIT ( * ) PLANE_ANGLE_UNIT ( ) SI_UNIT ( $, .RADIAN. ) );
#6505 = CIRCLE ( 'NONE', #12129, 3.299999999999997158 ) ;
#6506 = EDGE_LOOP ( 'NONE', ( #8283, #5211 ) ) ;
#6507 = B_SPLINE_CURVE_WITH_KNOTS ( 'NONE', 3,
 ( #1304, #216, #13696, #4688 ),
 .UNSPECIFIED., .F., .F.,
 ( 4, 4 ),
 ( 2.380737581660915015E-07, 0.002336974151641525201 ),
 .UNSPECIFIED. ) ;
#6508 = CARTESIAN_POINT ( 'NONE',  ( 62.10586122665986863, -20.42344490663941414, -27.99999999999999645 ) ) ;
#6509 = EDGE_CURVE ( 'NONE', #9523, #1217, #11286, .T. ) ;
#6510 = CARTESIAN_POINT ( 'NONE',  ( 20.00000000000000711, 20.00000000000000355, -25.00000000000000000 ) ) ;
#6511 = DIRECTION ( 'NONE',  ( 0.000000000000000000, 0.000000000000000000, -1.000000000000000000 ) ) ;
#6512 = CARTESIAN_POINT ( 'NONE',  ( 6.800000000000084199, 4.618802153517023612, -1.387778780781445676E-14 ) ) ;
#6513 = CIRCLE ( 'NONE', #2097, 5.560781378645576645 ) ;
#6514 = DIRECTION ( 'NONE',  ( -1.000000000000000000, 0.000000000000000000, 0.000000000000000000 ) ) ;
#6515 = DIRECTION ( 'NONE',  ( 0.000000000000000000, 1.000000000000000000, 0.000000000000000000 ) ) ;
#6516 = CARTESIAN_POINT ( 'NONE',  ( 59.18121602037099649, 13.58289998256015352, 25.00000000000000000 ) ) ;
#6517 = CARTESIAN_POINT ( 'NONE',  ( -129.3408537872145132, 199.5765550933606107, -13.99999999999998401 ) ) ;
#6518 = FACE_BOUND ( 'NONE', #7040, .T. ) ;
#6519 = VECTOR ( 'NONE', #12795, 1000.000000000000000 ) ;
#6520 =( LENGTH_UNIT ( ) NAMED_UNIT ( * ) SI_UNIT ( .MILLI., .METRE. ) );
#6521 = DIRECTION ( 'NONE',  ( -1.000000000000000000, -1.665334536937734071E-16, -0.000000000000000000 ) ) ;
#6522 = ORIENTED_EDGE ( 'NONE', *, *, #13271, .F. ) ;
#6523 = CARTESIAN_POINT ( 'NONE',  ( -4.000000000000000000, -2.309401076758511806, -4.699999999999981526 ) ) ;
#6524 = DIRECTION ( 'NONE',  ( 0.000000000000000000, 0.000000000000000000, 1.000000000000000000 ) ) ;
#6525 = VECTOR ( 'NONE', #2108, 1000.000000000000000 ) ;
#6526 = EDGE_CURVE ( 'NONE', #10492, #6248, #1261, .T. ) ;
#6527 = ORIENTED_EDGE ( 'NONE', *, *, #13995, .F. ) ;
#6528 = DIRECTION ( 'NONE',  ( -1.000000000000000000, 0.000000000000000000, 0.000000000000000000 ) ) ;
#6529 =( BOUNDED_SURFACE ( )  B_SPLINE_SURFACE ( 3, 2, ( 
 ( #2552, #12293, #1237 ),
 ( #13758, #12503, #1369 ),
 ( #3444, #2269, #5686 ),
 ( #10162, #145, #13543 ),
 ( #3515, #5898, #6714 ),
 ( #5816, #2408, #6867 ) ),
 .UNSPECIFIED., .F., .F., .F. ) 
 B_SPLINE_SURFACE_WITH_KNOTS ( ( 4, 2, 4 ),
 ( 3, 3 ),
 ( 0.02023740217035200836, 0.02269762987400599646, 0.02515785757765998457 ),
 ( 0.000000000000000000, 1.000000000000000000 ),
 .UNSPECIFIED. ) 
 GEOMETRIC_REPRESENTATION_ITEM ( )  RATIONAL_B_SPLINE_SURFACE ( (
 ( 1.000000000000000000, 0.8047781539129729156, 1.000000000000000000),
 ( 1.000000000000000000, 0.8123770319056065059, 1.000000000000000000),
 ( 1.000000000000000000, 0.8190663783058289571, 1.000000000000000000),
 ( 1.000000000000000000, 0.8192359702875615657, 1.000000000000000000),
 ( 1.000000000000000000, 0.8126134888420907254, 1.000000000000000000),
 ( 1.000000000000000000, 0.8047712368238109093, 1.000000000000000000) ) ) 
 REPRESENTATION_ITEM ( '' )  SURFACE ( )  );
#6530 = CARTESIAN_POINT ( 'NONE',  ( 0.000000000000000000, 0.000000000000000000, 0.000000000000000000 ) ) ;
#6531 = VERTEX_POINT ( 'NONE', #441 ) ;
#6532 = VERTEX_POINT ( 'NONE', #12725 ) ;
#6533 = DIRECTION ( 'NONE',  ( -1.000000000000000000, 1.892425610156516875E-16, 0.000000000000000000 ) ) ;
#6534 = CARTESIAN_POINT ( 'NONE',  ( 3.951447005078477126, -2.357513599190964371, 2.916666666666658081 ) ) ;
#6535 = LINE ( 'NONE', #3198, #489 ) ;
#6536 = LINE ( 'NONE', #910, #12178 ) ;
#6537 = CIRCLE ( 'NONE', #5825, 5.000000000000018652 ) ;
#6538 = DIRECTION ( 'NONE',  ( 0.000000000000000000, 0.000000000000000000, -1.000000000000000000 ) ) ;
#6539 = ADVANCED_FACE ( 'NONE', ( #4970 ), #10530, .T. ) ;
#6540 = CARTESIAN_POINT ( 'NONE',  ( 0.000000000000000000, 0.000000000000000000, -3.699999999999981082 ) ) ;
#6541 = EDGE_LOOP ( 'NONE', ( #1455, #9982, #10857, #2955 ) ) ;
#6542 =( NAMED_UNIT ( * ) PLANE_ANGLE_UNIT ( ) SI_UNIT ( $, .RADIAN. ) );
#6543 = CARTESIAN_POINT ( 'NONE',  ( -2.714587707229014324, 4.206234748388740563, -3.210254870093797102E-15 ) ) ;
#6544 = ADVANCED_FACE ( 'NONE', ( #1828 ), #5326, .T. ) ;
#6545 = DIRECTION ( 'NONE',  ( 0.000000000000000000, 0.000000000000000000, 1.000000000000000000 ) ) ;
#6546 = AXIS2_PLACEMENT_3D ( 'NONE', #7063, #2402, #12496 ) ;
#6547 = VECTOR ( 'NONE', #9873, 1000.000000000000000 ) ;
#6548 = VERTEX_POINT ( 'NONE', #4117 ) ;
#6549 = VERTEX_POINT ( 'NONE', #4256 ) ;
#6550 = AXIS2_PLACEMENT_3D ( 'NONE', #9311, #5065, #14015 ) ;
#6551 = ORIENTED_EDGE ( 'NONE', *, *, #5991, .T. ) ;
#6552 = DIRECTION ( 'NONE',  ( 0.000000000000000000, 0.000000000000000000, -1.000000000000000000 ) ) ;
#6553 = VERTEX_POINT ( 'NONE', #802 ) ;
#6554 = DIRECTION ( 'NONE',  ( 1.000000000000000000, 0.000000000000000000, 0.000000000000000000 ) ) ;
#6555 = DIRECTION ( 'NONE',  ( -1.000000000000000000, 0.000000000000000000, 0.000000000000000000 ) ) ;
#6556 = DIRECTION ( 'NONE',  ( 0.000000000000000000, 0.000000000000000000, -1.000000000000000000 ) ) ;
#6557 = ADVANCED_FACE ( 'NONE', ( #6278 ), #10751, .F. ) ;
#6558 = AXIS2_PLACEMENT_3D ( 'NONE', #2340, #11267, #1243 ) ;
#6559 = DIRECTION ( 'NONE',  ( 0.000000000000000000, 8.482162385747133845E-47, -1.000000000000000000 ) ) ;
#6560 = PRESENTATION_LAYER_ASSIGNMENT (  '', '', ( #4704 ) ) ;
#6561 = ORIENTED_EDGE ( 'NONE', *, *, #967, .T. ) ;
#6562 = CARTESIAN_POINT ( 'NONE',  ( 4.050536630291714069, 3.778525289263168219, 0.5912575323401301208 ) ) ;
#6563 = CARTESIAN_POINT ( 'NONE',  ( 4.024499207728660544, -2.323545700935590652, -3.272172305156503480 ) ) ;
#6564 = VECTOR ( 'NONE', #682, 1000.000000000000000 ) ;
#6565 = CARTESIAN_POINT ( 'NONE',  ( 4.175572532730952524, 2.061029303918050282, -3.569807470274386496 ) ) ;
#6566 = ORIENTED_EDGE ( 'NONE', *, *, #7378, .F. ) ;
#6567 = CARTESIAN_POINT ( 'NONE',  ( -3.081487911019577365E-30, 3.469446951953614189E-15, -5.974599999999997024 ) ) ;
#6568 = ORIENTED_EDGE ( 'NONE', *, *, #12402, .F. ) ;
#6569 = VECTOR ( 'NONE', #13181, 1000.000000000000000 ) ;
#6570 = AXIS2_PLACEMENT_3D ( 'NONE', #3392, #7828, #2137 ) ;
#6571 = CARTESIAN_POINT ( 'NONE',  ( 5.103531824934226080, -2.354098498486466351, -4.077418205400154427 ) ) ;
#6572 = ORIENTED_EDGE ( 'NONE', *, *, #5957, .T. ) ;
#6573 = FACE_OUTER_BOUND ( 'NONE', #1570, .T. ) ;
#6574 = DIRECTION ( 'NONE',  ( 1.734723475976770502E-18, -4.440892098500621231E-16, -1.000000000000000000 ) ) ;
#6575 = LINE ( 'NONE', #4197, #13326 ) ;
#6576 = EDGE_CURVE ( 'NONE', #3917, #4711, #12968, .T. ) ;
#6577 = DIRECTION ( 'NONE',  ( 0.000000000000000000, 5.551115123125782702E-17, 1.000000000000000000 ) ) ;
#6578 = VERTEX_POINT ( 'NONE', #1975 ) ;
#6579 = FACE_OUTER_BOUND ( 'NONE', #905, .T. ) ;
#6580 = DIRECTION ( 'NONE',  ( 1.000000000000000000, -0.000000000000000000, -0.000000000000000000 ) ) ;
#6581 = CIRCLE ( 'NONE', #8205, 2.100000000000000977 ) ;
#6582 = CARTESIAN_POINT ( 'NONE',  ( 22.00000000000000000, 80.00000000000000000, 25.00000000000000000 ) ) ;
#6583 = ORIENTED_EDGE ( 'NONE', *, *, #6494, .F. ) ;
#6584 = VECTOR ( 'NONE', #1248, 1000.000000000000000 ) ;
#6585 = VECTOR ( 'NONE', #6136, 1000.000000000000000 ) ;
#6586 = ORIENTED_EDGE ( 'NONE', *, *, #6493, .T. ) ;
#6587 = DIRECTION ( 'NONE',  ( 0.000000000000000000, 1.000000000000000000, 0.000000000000000000 ) ) ;
#6588 = CARTESIAN_POINT ( 'NONE',  ( 0.000000000000000000, 19.49999999999999645, 0.000000000000000000 ) ) ;
#6589 = CARTESIAN_POINT ( 'NONE',  ( 2.749999999999997780, 25.49999999999996803, 8.000000000000007105 ) ) ;
#6590 = LINE ( 'NONE', #5635, #2367 ) ;
#6591 = VECTOR ( 'NONE', #2280, 1000.000000000000000 ) ;
#6592 = AXIS2_PLACEMENT_3D ( 'NONE', #4196, #3098, #7528 ) ;
#6593 = DIRECTION ( 'NONE',  ( -1.000000000000000000, 0.000000000000000000, 0.000000000000000000 ) ) ;
#6594 = CARTESIAN_POINT ( 'NONE',  ( 0.000000000000000000, 189.5765550933606107, 33.00000000000002842 ) ) ;
#6595 = DIRECTION ( 'NONE',  ( -0.000000000000000000, -0.000000000000000000, -1.000000000000000000 ) ) ;
#6596 = EDGE_CURVE ( 'NONE', #11965, #13646, #14061, .T. ) ;
#6597 = DIRECTION ( 'NONE',  ( 0.000000000000000000, -0.000000000000000000, 1.000000000000000000 ) ) ;
#6598 = EDGE_CURVE ( 'NONE', #9365, #6262, #1615, .T. ) ;
#6599 = FILL_AREA_STYLE ('',( #1860 ) ) ;
#6600 = CARTESIAN_POINT ( 'NONE',  ( 5.024612689793094944, 2.312654742478284398, 4.005635514337482661 ) ) ;
#6601 = ORIENTED_EDGE ( 'NONE', *, *, #5913, .F. ) ;
#6602 = VERTEX_POINT ( 'NONE', #2036 ) ;
#6603 = CARTESIAN_POINT ( 'NONE',  ( 4.071447262713911996, -4.041451884327377009, 0.000000000000000000 ) ) ;
#6604 = CIRCLE ( 'NONE', #10819, 5.560781378645576645 ) ;
#6605 = ORIENTED_EDGE ( 'NONE', *, *, #6596, .T. ) ;
#6606 = CARTESIAN_POINT ( 'NONE',  ( 20.00000000000000000, -5.510910596163090344E-15, 25.00000000000000000 ) ) ;
#6607 = DIRECTION ( 'NONE',  ( 0.000000000000000000, 0.000000000000000000, 1.000000000000000000 ) ) ;
#6608 = ORIENTED_EDGE ( 'NONE', *, *, #5681, .F. ) ;
#6609 = FACE_OUTER_BOUND ( 'NONE', #9466, .T. ) ;
#6610 = CARTESIAN_POINT ( 'NONE',  ( 54.33050351964436686, 32.98574998546678927, -25.00000000000000000 ) ) ;
#6611 = CARTESIAN_POINT ( 'NONE',  ( 0.000000000000000000, 0.000000000000000000, 0.000000000000000000 ) ) ;
#6612 = AXIS2_PLACEMENT_3D ( 'NONE', #11806, #11950, #7604 ) ;
#6613 = CARTESIAN_POINT ( 'NONE',  ( 54.35294117647056567, -1.411764705882362358, 23.00000000000000000 ) ) ;
#6614 = EDGE_CURVE ( 'NONE', #11486, #6243, #2802, .T. ) ;
#6615 = EDGE_CURVE ( 'NONE', #1693, #14098, #6466, .T. ) ;
#6616 = CARTESIAN_POINT ( 'NONE',  ( -2.369796611257730795E-32, -4.618802153517031606, -3.204271511726780375 ) ) ;
#6617 = CARTESIAN_POINT ( 'NONE',  ( 33.99999999999998579, 80.00000000000000000, -23.00000000000000000 ) ) ;
#6618 = EDGE_LOOP ( 'NONE', ( #9153, #3839, #7471, #13395 ) ) ;
#6619 = VECTOR ( 'NONE', #11261, 1000.000000000000114 ) ;
#6620 = EDGE_CURVE ( 'NONE', #13071, #6239, #2564, .T. ) ;
#6621 = LINE ( 'NONE', #10063, #2071 ) ;
#6622 = LINE ( 'NONE', #4319, #3916 ) ;
#6623 = AXIS2_PLACEMENT_3D ( 'NONE', #12648, #1379, #8184 ) ;
#6624 = EDGE_CURVE ( 'NONE', #1788, #10504, #6294, .T. ) ;
#6625 = ORIENTED_EDGE ( 'NONE', *, *, #4663, .T. ) ;
#6626 = VERTEX_POINT ( 'NONE', #7648 ) ;
#6627 = AXIS2_PLACEMENT_3D ( 'NONE', #1129, #4584, #2167 ) ;
#6628 = CARTESIAN_POINT ( 'NONE',  ( 0.1381419387119249831, -1.355287006778807868, -3.499999999999996003 ) ) ;
#6629 = ORIENTED_EDGE ( 'NONE', *, *, #125, .T. ) ;
#6630 = CARTESIAN_POINT ( 'NONE',  ( 4.055487192203054647, 1.409979666029696155, -3.568038521265871399 ) ) ;
#6631 = EDGE_CURVE ( 'NONE', #14193, #937, #1008, .T. ) ;
#6632 = CARTESIAN_POINT ( 'NONE',  ( 56.99999999999997868, -8.673617379884035472E-16, -25.00000000000000000 ) ) ;
#6633 = EDGE_CURVE ( 'NONE', #13484, #10880, #13462, .T. ) ;
#6634 = CARTESIAN_POINT ( 'NONE',  ( 28.00000000000000355, 29.99999999999999645, -24.99999999999999289 ) ) ;
#6635 = DIRECTION ( 'NONE',  ( 0.000000000000000000, -4.440892098500620245E-16, -1.000000000000000000 ) ) ;
#6636 = VERTEX_POINT ( 'NONE', #5675 ) ;
#6637 = DIRECTION ( 'NONE',  ( -1.000000000000000000, 0.000000000000000000, 0.000000000000000000 ) ) ;
#6638 = CONTEXT_DEPENDENT_SHAPE_REPRESENTATION ( #3459, #8720 ) ;
#6639 = DIRECTION ( 'NONE',  ( 0.000000000000000000, -5.551115123125782702E-17, -1.000000000000000000 ) ) ;
#6640 = FACE_OUTER_BOUND ( 'NONE', #11690, .T. ) ;
#6641 = CLOSED_SHELL ( 'NONE', ( #3095, #377, #1691, #1622, #9393, #5316, #1825, #4074, #7709, #4333, #10182, #557, #9207, #7256 ) ) ;
#6642 = ORIENTED_EDGE ( 'NONE', *, *, #11882, .F. ) ;
#6643 = DIRECTION ( 'NONE',  ( -0.5000000000000042188, 0.000000000000000000, 0.8660254037844361541 ) ) ;
#6644 = ORIENTED_EDGE ( 'NONE', *, *, #4515, .F. ) ;
#6645 = EDGE_CURVE ( 'NONE', #6262, #9365, #13556, .T. ) ;
#6646 = ORIENTED_EDGE ( 'NONE', *, *, #10847, .T. ) ;
#6647 = ORIENTED_EDGE ( 'NONE', *, *, #14097, .F. ) ;
#6648 = EDGE_LOOP ( 'NONE', ( #11525, #9649, #3223, #1299, #5699 ) ) ;
#6649 = CARTESIAN_POINT ( 'NONE',  ( 2.000000000000001776, -3.464101615137764156, 0.000000000000000000 ) ) ;
#6650 = DIRECTION ( 'NONE',  ( -0.7071067811865513475, 3.141989118817382096E-16, 0.7071067811865437980 ) ) ;
#6651 = CYLINDRICAL_SURFACE ( 'NONE', #4459, 2.500000000000002220 ) ;
#6652 = DIRECTION ( 'NONE',  ( 1.000000000000000000, 0.000000000000000000, 0.000000000000000000 ) ) ;
#6653 = ORIENTED_EDGE ( 'NONE', *, *, #5207, .F. ) ;
#6654 = PLANE ( 'NONE',  #6694 ) ;
#6655 = DIRECTION ( 'NONE',  ( -0.8660254037844365982, 0.5000000000000036637, 9.625874682719161934E-32 ) ) ;
#6656 = CARTESIAN_POINT ( 'NONE',  ( 0.000000000000000000, 0.000000000000000000, 0.000000000000000000 ) ) ;
#6657 = CARTESIAN_POINT ( 'NONE',  ( 0.000000000000000000, 0.000000000000000000, 1.159999999999994369 ) ) ;
#6658 = ORIENTED_EDGE ( 'NONE', *, *, #12525, .T. ) ;
#6659 = LINE ( 'NONE', #6508, #8116 ) ;
#6660 = CYLINDRICAL_SURFACE ( 'NONE', #13857, 2.500000000000002220 ) ;
#6661 = EDGE_CURVE ( 'NONE', #14126, #11894, #12132, .T. ) ;
#6662 = LINE ( 'NONE', #4430, #13184 ) ;
#6663 = VERTEX_POINT ( 'NONE', #2110 ) ;
#6664 = DIRECTION ( 'NONE',  ( -1.000000000000000000, 0.000000000000000000, 0.000000000000000000 ) ) ;
#6665 = DIRECTION ( 'NONE',  ( 0.000000000000000000, 0.000000000000000000, -1.000000000000000000 ) ) ;
#6666 = CARTESIAN_POINT ( 'NONE',  ( 56.75585977000769589, 23.28432498401347672, 25.00000000000000000 ) ) ;
#6667 = ADVANCED_FACE ( 'NONE', ( #2191 ), #4469, .T. ) ;
#6668 = CARTESIAN_POINT ( 'NONE',  ( 129.3408537872138595, 189.5765550933606107, -69.99999999999998579 ) ) ;
#6669 = PRESENTATION_STYLE_ASSIGNMENT (( #2361 ) ) ;
#6670 = AXIS2_PLACEMENT_3D ( 'NONE', #11954, #13060, #3908 ) ;
#6671 = CARTESIAN_POINT ( 'NONE',  ( 5.005339938400140909, 2.401215914016161967, 4.000000000000002665 ) ) ;
#6672 = ORIENTED_EDGE ( 'NONE', *, *, #11672, .T. ) ;
#6673 = VERTEX_POINT ( 'NONE', #3505 ) ;
#6674 = DIRECTION ( 'NONE',  ( -8.619211990076296383E-16, 1.000000000000000000, 0.000000000000000000 ) ) ;
#6675 = B_SPLINE_CURVE_WITH_KNOTS ( 'NONE', 3,
 ( #3938, #11679, #416, #2766, #346, #6030 ),
 .UNSPECIFIED., .F., .F.,
 ( 4, 2, 4 ),
 ( 0.002336974151641525201, 0.003500975885716433710, 0.004664977619791342220 ),
 .UNSPECIFIED. ) ;
#6676 =( NAMED_UNIT ( * ) PLANE_ANGLE_UNIT ( ) SI_UNIT ( $, .RADIAN. ) );
#6677 = EDGE_LOOP ( 'NONE', ( #10115, #11411, #4113 ) ) ;
#6678 = EDGE_CURVE ( 'NONE', #131, #12036, #11918, .T. ) ;
#6679 = CARTESIAN_POINT ( 'NONE',  ( 0.2494252716035087192, 1.935831255942378926, 4.000000000000003553 ) ) ;
#6680 = ORIENTED_EDGE ( 'NONE', *, *, #6989, .T. ) ;
#6681 = EDGE_CURVE ( 'NONE', #9296, #2995, #7874, .T. ) ;
#6682 = VERTEX_POINT ( 'NONE', #9937 ) ;
#6683 = ORIENTED_EDGE ( 'NONE', *, *, #6831, .F. ) ;
#6684 = CARTESIAN_POINT ( 'NONE',  ( 6.938893903907228378E-15, 24.50000000000002132, 8.000000000000007105 ) ) ;
#6685 = LINE ( 'NONE', #13578, #3101 ) ;
#6686 = CARTESIAN_POINT ( 'NONE',  ( 4.086376042167605860, 1.979461949354207828, -3.571471332069182658 ) ) ;
#6687 = DIRECTION ( 'NONE',  ( 0.000000000000000000, 1.000000000000000000, 0.000000000000000000 ) ) ;
#6688 = CARTESIAN_POINT ( 'NONE',  ( 21.68170757442806362, 141.2731697022877313, -25.00000000000000000 ) ) ;
#6689 = CARTESIAN_POINT ( 'NONE',  ( 20.00000000000000355, 17.00000000000000000, -25.00000000000000000 ) ) ;
#6690 = ORIENTED_EDGE ( 'NONE', *, *, #4773, .T. ) ;
#6691 = ORIENTED_EDGE ( 'NONE', *, *, #13993, .F. ) ;
#6692 = CARTESIAN_POINT ( 'NONE',  ( -4.598786737361986177, 3.118391931134631978, -0.4203182062997263824 ) ) ;
#6693 = CARTESIAN_POINT ( 'NONE',  ( -3.065261730689029740, 7.410293710401353984, 0.000000000000000000 ) ) ;
#6694 = AXIS2_PLACEMENT_3D ( 'NONE', #3235, #4277, #12152 ) ;
#6695 = ORIENTED_EDGE ( 'NONE', *, *, #7933, .T. ) ;
#6696 = EDGE_LOOP ( 'NONE', ( #13422, #4781, #6245, #9411 ) ) ;
#6697 = VERTEX_POINT ( 'NONE', #5471 ) ;
#6698 = DIRECTION ( 'NONE',  ( 0.000000000000000000, 0.000000000000000000, 1.000000000000000000 ) ) ;
#6699 = ORIENTED_EDGE ( 'NONE', *, *, #3581, .F. ) ;
#6700 = CARTESIAN_POINT ( 'NONE',  ( 54.35294117647056567, -1.411764705882362358, -25.00000000000000000 ) ) ;
#6701 = DIRECTION ( 'NONE',  ( -1.000000000000000000, 0.000000000000000000, 0.000000000000000000 ) ) ;
#6702 = EDGE_LOOP ( 'NONE', ( #11336, #13291 ) ) ;
#6703 = DIRECTION ( 'NONE',  ( -0.9701425001453319874, -0.2425356250363327471, 0.000000000000000000 ) ) ;
#6704 = CARTESIAN_POINT ( 'NONE',  ( 30.10000000000000497, 29.99999999999999645, 6.999999999999992006 ) ) ;
#6705 = ORIENTED_EDGE ( 'NONE', *, *, #12218, .T. ) ;
#6706 = CARTESIAN_POINT ( 'NONE',  ( 54.35294117647056567, -1.411764705882362358, 25.00000000000000000 ) ) ;
#6707 = CONTEXT_DEPENDENT_SHAPE_REPRESENTATION ( #8766, #9160 ) ;
#6708 = DIRECTION ( 'NONE',  ( 0.000000000000000000, 0.000000000000000000, 1.000000000000000000 ) ) ;
#6709 = DIRECTION ( 'NONE',  ( -0.000000000000000000, -0.000000000000000000, -1.000000000000000000 ) ) ;
#6710 = CIRCLE ( 'NONE', #13738, 0.7999999999999999334 ) ;
#6711 = CARTESIAN_POINT ( 'NONE',  ( 4.630153689607063860, 9.559099815976924059E-16, 5.371010071662830399 ) ) ;
#6712 = ADVANCED_FACE ( 'NONE', ( #10006 ), #14410, .T. ) ;
#6713 = ORIENTED_EDGE ( 'NONE', *, *, #12716, .T. ) ;
#6714 = CARTESIAN_POINT ( 'NONE',  ( -3.522881874162831828, 2.820349071481866421, -3.298443181296048188 ) ) ;
#6715 = EDGE_LOOP ( 'NONE', ( #12736, #854, #1416, #9331 ) ) ;
#6716 = VECTOR ( 'NONE', #8049, 1000.000000000000000 ) ;
#6717 = ORIENTED_EDGE ( 'NONE', *, *, #11567, .T. ) ;
#6718 = VECTOR ( 'NONE', #803, 1000.000000000000000 ) ;
#6719 = FACE_OUTER_BOUND ( 'NONE', #3825, .T. ) ;
#6720 = CARTESIAN_POINT ( 'NONE',  ( -2.179555516819069894, 4.788648424347440979, -4.357628883416061250 ) ) ;
#6721 = CARTESIAN_POINT ( 'NONE',  ( -5.000000000000000000, 3.130593237335734802, -4.327781269827185362 ) ) ;
#6722 = LINE ( 'NONE', #5486, #1899 ) ;
#6723 = ORIENTED_EDGE ( 'NONE', *, *, #3619, .T. ) ;
#6724 = CARTESIAN_POINT ( 'NONE',  ( 71.80728622811317052, -17.99808865627607801, 25.00000000000000000 ) ) ;
#6725 = DIRECTION ( 'NONE',  ( 0.000000000000000000, -0.000000000000000000, 1.000000000000000000 ) ) ;
#6726 = DIRECTION ( 'NONE',  ( 0.000000000000000000, 0.000000000000000000, 1.000000000000000000 ) ) ;
#6727 = ADVANCED_FACE ( 'NONE', ( #3369 ), #7548, .T. ) ;
#6728 = LINE ( 'NONE', #6582, #10080 ) ;
#6729 = ORIENTED_EDGE ( 'NONE', *, *, #1371, .F. ) ;
#6730 = EDGE_LOOP ( 'NONE', ( #12509, #1221 ) ) ;
#6731 = AXIS2_PLACEMENT_3D ( 'NONE', #14436, #12025, #4283 ) ;
#6732 = DIRECTION ( 'NONE',  ( 0.000000000000000000, 0.000000000000000000, 1.000000000000000000 ) ) ;
#6733 = CIRCLE ( 'NONE', #2300, 5.384454397937120440 ) ;
#6734 = FACE_BOUND ( 'NONE', #14243, .T. ) ;
#6735 = EDGE_CURVE ( 'NONE', #9330, #1788, #4604, .T. ) ;
#6736 = CONICAL_SURFACE ( 'NONE', #9303, 3.499999999999999112, 1.047197551196600296 ) ;
#6737 = LINE ( 'NONE', #14368, #6146 ) ;
#6738 = CARTESIAN_POINT ( 'NONE',  ( 20.00000000000000000, 70.00000000000000000, 25.00000000000000000 ) ) ;
#6739 = PRODUCT_DEFINITION_CONTEXT ( 'detailed design', #10449, 'design' ) ;
#6740 = DIRECTION ( 'NONE',  ( 0.000000000000000000, 0.000000000000000000, -1.000000000000000000 ) ) ;
#6741 = FACE_OUTER_BOUND ( 'NONE', #8783, .T. ) ;
#6742 = STYLED_ITEM ( 'NONE', ( #347 ), #6797 ) ;
#6743 = DIRECTION ( 'NONE',  ( 0.000000000000000000, 0.000000000000000000, -1.000000000000000000 ) ) ;
#6744 = ADVANCED_FACE ( 'NONE', ( #2259 ), #12351, .F. ) ;
#6745 = CARTESIAN_POINT ( 'NONE',  ( 4.050536630291718510, -3.778525289263177989, -0.5912575323401209060 ) ) ;
#6746 = ORIENTED_EDGE ( 'NONE', *, *, #12141, .T. ) ;
#6747 = DIRECTION ( 'NONE',  ( -2.243905293393255080E-15, 8.975621173573017164E-15, 1.000000000000000000 ) ) ;
#6748 = ORIENTED_EDGE ( 'NONE', *, *, #10141, .T. ) ;
#6749 = DIRECTION ( 'NONE',  ( -0.000000000000000000, -1.000000000000000000, 0.000000000000000000 ) ) ;
#6750 = ORIENTED_EDGE ( 'NONE', *, *, #4339, .F. ) ;
#6751 = PLANE ( 'NONE',  #1033 ) ;
#6752 = CARTESIAN_POINT ( 'NONE',  ( 58.68170757442803165, 39.57655509336063204, -33.00000000000000000 ) ) ;
#6753 = CARTESIAN_POINT ( 'NONE',  ( 4.030867648404682591, -3.732851566702919843, -0.5345114293595707444 ) ) ;
#6754 = CARTESIAN_POINT ( 'NONE',  ( -28.00000000000000355, 35.49999999999997868, 8.000000000000007105 ) ) ;
#6755 =( NAMED_UNIT ( * ) PLANE_ANGLE_UNIT ( ) SI_UNIT ( $, .RADIAN. ) );
#6756 = EDGE_CURVE ( 'NONE', #1060, #8772, #2324, .T. ) ;
#6757 = CARTESIAN_POINT ( 'NONE',  ( 3.000000000000000888, 3.836840991697820422E-15, -5.974599999999997024 ) ) ;
#6758 = ORIENTED_EDGE ( 'NONE', *, *, #4501, .T. ) ;
#6759 = EDGE_CURVE ( 'NONE', #12258, #2748, #6513, .T. ) ;
#6760 = LINE ( 'NONE', #5719, #5620 ) ;
#6761 = CONICAL_SURFACE ( 'NONE', #9809, 4.000000000000004441, 1.047197551196600296 ) ;
#6762 = VERTEX_POINT ( 'NONE', #9039 ) ;
#6763 = LINE ( 'NONE', #7636, #7912 ) ;
#6764 = CONICAL_SURFACE ( 'NONE', #10516, 4.000000000000004441, 1.047197551196600296 ) ;
#6765 = CARTESIAN_POINT ( 'NONE',  ( 4.158806965674299860, 1.986429158307079224, 3.559403772175830927 ) ) ;
#6766 = EDGE_LOOP ( 'NONE', ( #6653, #9405 ) ) ;
#6767 = MANIFOLD_SOLID_BREP ( 'AdvancedHole1', #5700 ) ;
#6768 = ORIENTED_EDGE ( 'NONE', *, *, #14124, .F. ) ;
#6769 = ORIENTED_EDGE ( 'NONE', *, *, #8768, .T. ) ;
#6770 = AXIS2_PLACEMENT_3D ( 'NONE', #13030, #3080, #4177 ) ;
#6771 = CARTESIAN_POINT ( 'NONE',  ( 0.1578711657484770381, -1.548887424832829707, -4.000000000000002665 ) ) ;
#6772 = VERTEX_POINT ( 'NONE', #11602 ) ;
#6773 = DIRECTION ( 'NONE',  ( -0.000000000000000000, 8.482162385747133845E-47, -1.000000000000000000 ) ) ;
#6774 = CARTESIAN_POINT ( 'NONE',  ( -2.000000000000001776, -3.464101615137750390, 0.000000000000000000 ) ) ;
#6775 = CARTESIAN_POINT ( 'NONE',  ( 20.00000000000000355, 40.00000000000000711, 25.00000000000000000 ) ) ;
#6776 = EDGE_CURVE ( 'NONE', #9291, #3573, #3288, .T. ) ;
#6777 = DIRECTION ( 'NONE',  ( 2.273843122241273031E-18, -2.220446049250313574E-16, 1.000000000000000000 ) ) ;
#6778 = EDGE_CURVE ( 'NONE', #3711, #4424, #1516, .T. ) ;
#6779 = DIRECTION ( 'NONE',  ( 0.000000000000000000, 0.000000000000000000, -1.000000000000000000 ) ) ;
#6780 = CONTEXT_DEPENDENT_SHAPE_REPRESENTATION ( #5948, #303 ) ;
#6781 = CARTESIAN_POINT ( 'NONE',  ( 76.68170757442796059, 3.003422806631532356E-13, -33.00000000000000000 ) ) ;
#6782 = CARTESIAN_POINT ( 'NONE',  ( 5.067058822021065723, -4.651083900313782493, -1.401471914501746383E-14 ) ) ;
#6783 = CIRCLE ( 'NONE', #1888, 3.299999999999997158 ) ;
#6784 = AXIS2_PLACEMENT_3D ( 'NONE', #6962, #7108, #10412 ) ;
#6785 = AXIS2_PLACEMENT_3D ( 'NONE', #8857, #4002, #6664 ) ;
#6786 = FACE_BOUND ( 'NONE', #7453, .T. ) ;
#6787 = ORIENTED_EDGE ( 'NONE', *, *, #14125, .F. ) ;
#6788 = ORIENTED_EDGE ( 'NONE', *, *, #1962, .T. ) ;
#6789 = DIRECTION ( 'NONE',  ( 0.000000000000000000, -1.000000000000000000, 0.000000000000000000 ) ) ;
#6790 = EDGE_LOOP ( 'NONE', ( #10676, #9145, #9254, #9026 ) ) ;
#6791 = VECTOR ( 'NONE', #11769, 1000.000000000000000 ) ;
#6792 = ORIENTED_EDGE ( 'NONE', *, *, #8769, .T. ) ;
#6793 =( NAMED_UNIT ( * ) SI_UNIT ( $, .STERADIAN. ) SOLID_ANGLE_UNIT ( ) );
#6794 = VECTOR ( 'NONE', #7268, 1000.000000000000114 ) ;
#6795 = LINE ( 'NONE', #12368, #5394 ) ;
#6796 =( NAMED_UNIT ( * ) PLANE_ANGLE_UNIT ( ) SI_UNIT ( $, .RADIAN. ) );
#6797 = MANIFOLD_SOLID_BREP ( 'Cut-Extrude4', #2436 ) ;
#6798 = VECTOR ( 'NONE', #2429, 1000.000000000000000 ) ;
#6799 = CARTESIAN_POINT ( 'NONE',  ( 2.687328764639632883, -3.067272167851310627, -0.05923475698271751799 ) ) ;
#6800 = PLANE ( 'NONE',  #14190 ) ;
#6801 = EDGE_CURVE ( 'NONE', #3003, #2985, #6108, .T. ) ;
#6802 = FACE_OUTER_BOUND ( 'NONE', #5241, .T. ) ;
#6803 =( LENGTH_UNIT ( ) NAMED_UNIT ( * ) SI_UNIT ( .MILLI., .METRE. ) );
#6804 = EDGE_CURVE ( 'NONE', #9644, #13416, #3648, .T. ) ;
#6805 = VERTEX_POINT ( 'NONE', #3794 ) ;
#6806 = EDGE_CURVE ( 'NONE', #5220, #9041, #13896, .T. ) ;
#6807 = CARTESIAN_POINT ( 'NONE',  ( -8.000000000000000000, 25.49999999999996803, 8.000000000000007105 ) ) ;
#6808 = VECTOR ( 'NONE', #6934, 1000.000000000000000 ) ;
#6809 = VECTOR ( 'NONE', #13920, 1000.000000000000000 ) ;
#6810 = DIRECTION ( 'NONE',  ( 0.000000000000000000, 0.000000000000000000, 1.000000000000000000 ) ) ;
#6811 = EDGE_LOOP ( 'NONE', ( #2780, #2121, #12059, #2521 ) ) ;
#6812 = VERTEX_POINT ( 'NONE', #4742 ) ;
#6813 = EDGE_CURVE ( 'NONE', #9740, #5462, #10590, .T. ) ;
#6814 = CARTESIAN_POINT ( 'NONE',  ( 4.859329672868200944, -2.661112198169292231, 3.390818468129448870 ) ) ;
#6815 = FACE_OUTER_BOUND ( 'NONE', #13835, .T. ) ;
#6816 = VECTOR ( 'NONE', #8744, 1000.000000000000000 ) ;
#6817 = FACE_OUTER_BOUND ( 'NONE', #13441, .T. ) ;
#6818 = VECTOR ( 'NONE', #13418, 1000.000000000000000 ) ;
#6819 = CIRCLE ( 'NONE', #11029, 2.100000000000000977 ) ;
#6820 = EDGE_CURVE ( 'NONE', #9459, #29, #5886, .T. ) ;
#6821 = EDGE_CURVE ( 'NONE', #7189, #3625, #12623, .T. ) ;
#6822 = CARTESIAN_POINT ( 'NONE',  ( 5.108576227836145733, -2.381533865848265208, 4.077513078102846578 ) ) ;
#6823 = ORIENTED_EDGE ( 'NONE', *, *, #13424, .T. ) ;
#6824 = DIRECTION ( 'NONE',  ( 1.000000000000000000, 1.913084959030911013E-15, 0.000000000000000000 ) ) ;
#6825 = FILL_AREA_STYLE_COLOUR ( '', #11491 ) ;
#6826 = VERTEX_POINT ( 'NONE', #6916 ) ;
#6827 = CARTESIAN_POINT ( 'NONE',  ( -5.736770013510187597E-15, -3.375361811986495653, 1.153701847711628536 ) ) ;
#6828 = VECTOR ( 'NONE', #13116, 1000.000000000000000 ) ;
#6829 = PRODUCT_DEFINITION_SHAPE ( 'NONE', 'NONE',  #11417 ) ;
#6830 = ORIENTED_EDGE ( 'NONE', *, *, #1282, .T. ) ;
#6831 = EDGE_CURVE ( 'NONE', #5807, #11937, #8841, .T. ) ;
#6832 = CARTESIAN_POINT ( 'NONE',  ( -24.99999999999998934, -30.42444490663959300, -2.000000000000001776 ) ) ;
#6833 = LINE ( 'NONE', #11299, #12432 ) ;
#6834 = FACE_OUTER_BOUND ( 'NONE', #837, .T. ) ;
#6835 = CARTESIAN_POINT ( 'NONE',  ( 0.000000000000000000, 0.000000000000000000, 0.000000000000000000 ) ) ;
#6836 = DIRECTION ( 'NONE',  ( -0.000000000000000000, 1.000000000000000000, -0.000000000000000000 ) ) ;
#6837 =( GEOMETRIC_REPRESENTATION_CONTEXT ( 3 ) GLOBAL_UNCERTAINTY_ASSIGNED_CONTEXT ( ( #3687 ) ) GLOBAL_UNIT_ASSIGNED_CONTEXT ( ( #4854, #10918, #12099 ) ) REPRESENTATION_CONTEXT ( 'NONE', 'WORKASPACE' ) );
#6838 = CARTESIAN_POINT ( 'NONE',  ( 5.103531824934171013, 4.708196996972911386, -1.387778780781445676E-14 ) ) ;
#6839 = CONICAL_SURFACE ( 'NONE', #13404, 4.000000000000000000, 0.8911886515913775009 ) ;
#6840 = ORIENTED_EDGE ( 'NONE', *, *, #5569, .F. ) ;
#6841 = DIRECTION ( 'NONE',  ( 0.000000000000000000, 0.000000000000000000, -1.000000000000000000 ) ) ;
#6842 = B_SPLINE_CURVE_WITH_KNOTS ( 'NONE', 3,
 ( #2991, #7489, #7285, #7360, #6333, #11835, #11677, #3936, #8534, #8597, #786, #8673, #14115, #13084, #7207, #9491 ),
 .UNSPECIFIED., .F., .F.,
 ( 4, 3, 3, 3, 3, 4 ),
 ( -2.111273352586108592E-06, 0.000000000000000000, 3.519286887797300651E-05, 7.191842652071138019E-05, 0.0001049868727093777871, 0.0001382836236822087195 ),
 .UNSPECIFIED. ) ;
#6843 = ORIENTED_EDGE ( 'NONE', *, *, #9210, .F. ) ;
#6844 = CARTESIAN_POINT ( 'NONE',  ( -5.000000000000001776, -2.886751345948152192, -4.284345921091780696 ) ) ;
#6845 = CARTESIAN_POINT ( 'NONE',  ( 3.958484000407669345, 3.734437307742072942, 0.5317648453099808048 ) ) ;
#6846 = ORIENTED_EDGE ( 'NONE', *, *, #2659, .T. ) ;
#6847 = ADVANCED_FACE ( 'NONE', ( #9262 ), #13746, .T. ) ;
#6848 = TOROIDAL_SURFACE ( 'NONE', #11292, 6.250000000000000000, 0.5499999999999992673 ) ;
#6849 = EDGE_LOOP ( 'NONE', ( #5156, #5596, #7420, #11471, #5132, #4533, #1487, #4884 ) ) ;
#6850 = CARTESIAN_POINT ( 'NONE',  ( 2.500000000000000444, 0.000000000000000000, -0.3501037691048258793 ) ) ;
#6851 = ORIENTED_EDGE ( 'NONE', *, *, #12017, .T. ) ;
#6852 = DIRECTION ( 'NONE',  ( -1.000000000000000000, 0.000000000000000000, 0.000000000000000000 ) ) ;
#6853 = VECTOR ( 'NONE', #8478, 1000.000000000000000 ) ;
#6854 = DIRECTION ( 'NONE',  ( 0.000000000000000000, 4.440892098500621231E-16, 1.000000000000000000 ) ) ;
#6855 = B_SPLINE_CURVE_WITH_KNOTS ( 'NONE', 3,
 ( #5906, #6937, #368, #12574 ),
 .UNSPECIFIED., .F., .F.,
 ( 4, 4 ),
 ( 2.380739282218358329E-07, 0.002044882221487521069 ),
 .UNSPECIFIED. ) ;
#6856 = FILL_AREA_STYLE ('',( #4669 ) ) ;
#6857 = PLANE ( 'NONE',  #14455 ) ;
#6858 = DIRECTION ( 'NONE',  ( -0.000000000000000000, 1.000000000000000000, -0.000000000000000000 ) ) ;
#6859 = AXIS2_PLACEMENT_3D ( 'NONE', #11271, #13419, #1249 ) ;
#6860 = CARTESIAN_POINT ( 'NONE',  ( -129.3408537872145132, 189.5765550933606107, -4.000000000000031086 ) ) ;
#6861 = CARTESIAN_POINT ( 'NONE',  ( 0.1586754815284894260, 2.687817229851479972, -3.344563996438210118 ) ) ;
#6862 = CARTESIAN_POINT ( 'NONE',  ( 5.000882498481283633, -4.618802153517009401, -2.416538104178194415E-20 ) ) ;
#6863 = VECTOR ( 'NONE', #10934, 1000.000000000000114 ) ;
#6864 = EDGE_CURVE ( 'NONE', #13172, #5863, #5107, .T. ) ;
#6865 = EDGE_CURVE ( 'NONE', #14145, #6982, #10665, .T. ) ;
#6866 = ORIENTED_EDGE ( 'NONE', *, *, #3370, .F. ) ;
#6867 = CARTESIAN_POINT ( 'NONE',  ( -4.236525418537980592, 2.416953631397924074, -3.451298686683611283 ) ) ;
#6868 = CARTESIAN_POINT ( 'NONE',  ( 22.00000000000000355, 40.00000000000000711, 25.00000000000000000 ) ) ;
#6869 = VERTEX_POINT ( 'NONE', #8536 ) ;
#6870 = VERTEX_POINT ( 'NONE', #6193 ) ;
#6871 = FACE_OUTER_BOUND ( 'NONE', #87, .T. ) ;
#6872 = DIRECTION ( 'NONE',  ( 0.2425356250363329969, -0.9701425001453318764, -0.000000000000000000 ) ) ;
#6873 = MANIFOLD_SOLID_BREP ( 'Boss-Extrude2', #6641 ) ;
#6874 = CARTESIAN_POINT ( 'NONE',  ( 22.00000000000000355, 50.00000000000000000, -25.00000000000000000 ) ) ;
#6875 = ADVANCED_FACE ( 'NONE', ( #11765 ), #12949, .F. ) ;
#6876 = VERTEX_POINT ( 'NONE', #9635 ) ;
#6877 = CARTESIAN_POINT ( 'NONE',  ( -31.44014396567295577, 21.68342561534834445, 0.000000000000000000 ) ) ;
#6878 = DIRECTION ( 'NONE',  ( 0.000000000000000000, 0.000000000000000000, 1.000000000000000000 ) ) ;
#6879 = DIRECTION ( 'NONE',  ( -0.9701425001453318764, -0.2425356250363329969, 0.000000000000000000 ) ) ;
#6880 = VERTEX_POINT ( 'NONE', #2845 ) ;
#6881 = CARTESIAN_POINT ( 'NONE',  ( 2.750000000000002665, 5.817072295949927426E-16, -4.750000000000000000 ) ) ;
#6882 = ORIENTED_EDGE ( 'NONE', *, *, #5100, .F. ) ;
#6883 = FACE_OUTER_BOUND ( 'NONE', #2369, .T. ) ;
#6884 = DIRECTION ( 'NONE',  ( 2.133709875451472726E-16, -1.000000000000000000, -0.000000000000000000 ) ) ;
#6885 =( NAMED_UNIT ( * ) PLANE_ANGLE_UNIT ( ) SI_UNIT ( $, .RADIAN. ) );
#6886 = LINE ( 'NONE', #4839, #6004 ) ;
#6887 = CARTESIAN_POINT ( 'NONE',  ( 5.013196232911383277, 2.310564645009324014, -4.002015359328510158 ) ) ;
#6888 = EDGE_LOOP ( 'NONE', ( #4191, #7370 ) ) ;
#6889 = CARTESIAN_POINT ( 'NONE',  ( 0.1597025669806160231, 1.557591170363314959, 4.000000000000003553 ) ) ;
#6890 = VERTEX_POINT ( 'NONE', #1811 ) ;
#6891 = ADVANCED_FACE ( 'NONE', ( #789 ), #5246, .F. ) ;
#6892 = ADVANCED_FACE ( 'NONE', ( #8461 ), #7959, .F. ) ;
#6893 = EDGE_LOOP ( 'NONE', ( #2823, #5754 ) ) ;
#6894 = FACE_OUTER_BOUND ( 'NONE', #1234, .T. ) ;
#6895 = FACE_OUTER_BOUND ( 'NONE', #3987, .T. ) ;
#6896 = AXIS2_PLACEMENT_3D ( 'NONE', #7688, #2068, #10985 ) ;
#6897 = CARTESIAN_POINT ( 'NONE',  ( 4.165266963751700580, -2.049631966911993786, -3.550066703508896637 ) ) ;
#6898 = CARTESIAN_POINT ( 'NONE',  ( 0.000000000000000000, 0.000000000000000000, 0.000000000000000000 ) ) ;
#6899 = CARTESIAN_POINT ( 'NONE',  ( 1.560000000000005826, -0.8660254037844428154, 1.500000000000001332 ) ) ;
#6900 = CARTESIAN_POINT ( 'NONE',  ( 3.951447005078475350, -1.347150628109120785, 3.499999999999988454 ) ) ;
#6901 = ORIENTED_EDGE ( 'NONE', *, *, #784, .T. ) ;
#6902 = LINE ( 'NONE', #11368, #13132 ) ;
#6903 = ORIENTED_EDGE ( 'NONE', *, *, #10923, .F. ) ;
#6904 = DIRECTION ( 'NONE',  ( 0.000000000000000000, -8.482162385747133845E-47, 1.000000000000000000 ) ) ;
#6905 = ADVANCED_FACE ( 'NONE', ( #6719 ), #4436, .T. ) ;
#6906 = ORIENTED_EDGE ( 'NONE', *, *, #10678, .T. ) ;
#6907 = DIRECTION ( 'NONE',  ( 1.000000000000000000, -0.000000000000000000, -0.000000000000000000 ) ) ;
#6909 = ORIENTED_EDGE ( 'NONE', *, *, #2055, .T. ) ;
#6908 = ADVANCED_FACE ( 'NONE', ( #6573 ), #13329, .T. ) ;
#6910 = MANIFOLD_SOLID_BREP ( 'EndChamfer', #12729 ) ;
#6911 = VERTEX_POINT ( 'NONE', #6649 ) ;
#6912 = DIRECTION ( 'NONE',  ( -2.273843122241289979E-18, 5.551115123125782702E-17, 1.000000000000000000 ) ) ;
#6913 = EDGE_LOOP ( 'NONE', ( #7247, #13358, #9406 ) ) ;
#6914 = DIRECTION ( 'NONE',  ( 0.000000000000000000, 0.8660254037844380415, -0.5000000000000012212 ) ) ;
#6915 = CARTESIAN_POINT ( 'NONE',  ( 5.000000000000001776, 2.068872943223520444, -4.395519625925073726 ) ) ;
#6916 = CARTESIAN_POINT ( 'NONE',  ( -8.000000000000000000, 25.49999999999996803, 8.000000000000007105 ) ) ;
#6917 = DIRECTION ( 'NONE',  ( 1.000000000000000000, 1.665334536937734318E-16, 0.000000000000000000 ) ) ;
#6918 = FACE_OUTER_BOUND ( 'NONE', #2754, .T. ) ;
#6919 = ITEM_DEFINED_TRANSFORMATION ( 'NONE', 'NONE', #10608,  #11025 ) ;
#6920 = DIRECTION ( 'NONE',  ( 1.000000000000000000, -0.000000000000000000, -0.000000000000000000 ) ) ;
#6921 = DIRECTION ( 'NONE',  ( 0.000000000000000000, 0.000000000000000000, 1.000000000000000000 ) ) ;
#6922 = ADVANCED_FACE ( 'NONE', ( #9952 ), #9310, .T. ) ;
#6923 = CARTESIAN_POINT ( 'NONE',  ( -1.734723475976807094E-14, 35.49999999999996447, 8.000000000000007105 ) ) ;
#6924 = AXIS2_PLACEMENT_3D ( 'NONE', #6666, #11205, #10986 ) ;
#6925 = EDGE_CURVE ( 'NONE', #6031, #12237, #14422, .T. ) ;
#6926 = ORIENTED_EDGE ( 'NONE', *, *, #11847, .F. ) ;
#6927 = LINE ( 'NONE', #2477, #2449 ) ;
#6928 = VERTEX_POINT ( 'NONE', #13411 ) ;
#6929 = VERTEX_POINT ( 'NONE', #8987 ) ;
#6930 = CARTESIAN_POINT ( 'NONE',  ( 0.000000000000000000, 0.000000000000000000, 0.000000000000000000 ) ) ;
#6931 = AXIS2_PLACEMENT_3D ( 'NONE', #11580, #1559, #8922 ) ;
#6932 = CARTESIAN_POINT ( 'NONE',  ( -7.055360934154693097E-15, -2.859595677584332307, 2.047034997319569172 ) ) ;
#6933 = CARTESIAN_POINT ( 'NONE',  ( -5.253679192976075107, 3.068494879228052419, -4.666070613310114190 ) ) ;
#6934 = DIRECTION ( 'NONE',  ( 0.000000000000000000, 0.000000000000000000, 1.000000000000000000 ) ) ;
#6935 = AXIS2_PLACEMENT_3D ( 'NONE', #9481, #4088, #4224 ) ;
#6936 = ORIENTED_EDGE ( 'NONE', *, *, #6804, .F. ) ;
#6937 = CARTESIAN_POINT ( 'NONE',  ( 0.1217565302851122550, 2.351289329882154888, 2.927447417349537950 ) ) ;
#6938 = DIRECTION ( 'NONE',  ( 1.000000000000000000, 0.000000000000000000, 0.000000000000000000 ) ) ;
#6939 = EDGE_CURVE ( 'NONE', #5249, #4147, #7820, .T. ) ;
#6940 = CARTESIAN_POINT ( 'NONE',  ( 79.68170757442804586, 124.5765550933606249, -25.00000000000000000 ) ) ;
#6941 = PRODUCT_DEFINITION ( 'UNKNOWN', '', #9435, #5985 ) ;
#6942 = ADVANCED_FACE ( 'NONE', ( #6871 ), #3230, .T. ) ;
#6943 = PRODUCT_DEFINITION_SHAPE ( 'NONE', 'NONE',  #14476 ) ;
#6944 = CARTESIAN_POINT ( 'NONE',  ( -5.236872748402765509, -8.016972670139777574E-14, -4.357689166958463645 ) ) ;
#6945 = EDGE_LOOP ( 'NONE', ( #9380, #9174, #9627, #11572 ) ) ;
#6946 = CIRCLE ( 'NONE', #666, 2.500000000000002220 ) ;
#6947 = AXIS2_PLACEMENT_3D ( 'NONE', #6868, #13107, #12000 ) ;
#6948 = ORIENTED_EDGE ( 'NONE', *, *, #3076, .T. ) ;
#6949 = ORIENTED_EDGE ( 'NONE', *, *, #11946, .T. ) ;
#6950 = CARTESIAN_POINT ( 'NONE',  ( -4.177163563997814114E-15, -5.807447148981907503, -4.451008977024222268 ) ) ;
#6951 = CARTESIAN_POINT ( 'NONE',  ( -2.500000000000000888, -1.101719344475952406E-16, -4.699999999999981526 ) ) ;
#6952 = CIRCLE ( 'NONE', #9055, 2.500000000000002220 ) ;
#6953 = EDGE_LOOP ( 'NONE', ( #5446, #10052, #10764, #13861 ) ) ;
#6954 = PLANE ( 'NONE',  #4863 ) ;
#6955 = CARTESIAN_POINT ( 'NONE',  ( 5.103531824934115946, 2.354098498486452584, 4.077418205400126894 ) ) ;
#6956 = ORIENTED_EDGE ( 'NONE', *, *, #9916, .T. ) ;
#6957 = LINE ( 'NONE', #8125, #3831 ) ;
#6958 = VERTEX_POINT ( 'NONE', #10093 ) ;
#6959 = VECTOR ( 'NONE', #9710, 1000.000000000000000 ) ;
#6960 = CARTESIAN_POINT ( 'NONE',  ( 1.560000000000005826, -0.8660254037844428154, 1.500000000000001332 ) ) ;
#6961 = CARTESIAN_POINT ( 'NONE',  ( 54.33050351964436686, 32.98574998546678927, -25.00000000000000000 ) ) ;
#6962 = CARTESIAN_POINT ( 'NONE',  ( 1.560000000000005826, -1.732050807568885631, 0.000000000000000000 ) ) ;
#6963 = FACE_OUTER_BOUND ( 'NONE', #9783, .T. ) ;
#6964 = CARTESIAN_POINT ( 'NONE',  ( -0.03111943836865819005, 6.084399642271183239, -4.666192694417976128 ) ) ;
#6965 = CARTESIAN_POINT ( 'NONE',  ( -1.721886139899573953, 5.052888355619120198, -4.357689166958383709 ) ) ;
#6966 = ORIENTED_EDGE ( 'NONE', *, *, #8646, .F. ) ;
#6967 = LINE ( 'NONE', #3698, #730 ) ;
#6968 = EDGE_CURVE ( 'NONE', #10480, #1551, #14241, .T. ) ;
#6969 = ORIENTED_EDGE ( 'NONE', *, *, #1730, .T. ) ;
#6970 = CARTESIAN_POINT ( 'NONE',  ( 6.123233995736773185E-16, -30.42444490663959300, -42.00000000000003553 ) ) ;
#6971 = CARTESIAN_POINT ( 'NONE',  ( 0.5449245075113242631, 4.304189842417321721, -3.016622336521755265 ) ) ;
#6972 = EDGE_LOOP ( 'NONE', ( #11494, #10908 ) ) ;
#6973 = CARTESIAN_POINT ( 'NONE',  ( 4.769962962079064894, -3.046916606660486693, -2.722585630838685766 ) ) ;
#6974 = ORIENTED_EDGE ( 'NONE', *, *, #12964, .F. ) ;
#6975 = CARTESIAN_POINT ( 'NONE',  ( 20.00000000000000000, -5.510910596163090344E-15, -25.00000000000000000 ) ) ;
#6976 = ORIENTED_EDGE ( 'NONE', *, *, #8145, .T. ) ;
#6977 = ORIENTED_EDGE ( 'NONE', *, *, #311, .T. ) ;
#6978 = CARTESIAN_POINT ( 'NONE',  ( 0.03363697881254360672, -0.7786124121997077818, -4.000000000000004441 ) ) ;
#6979 = CARTESIAN_POINT ( 'NONE',  ( 0.000000000000000000, -4.618802153517030717, -3.133295621305376422 ) ) ;
#6980 = B_SPLINE_CURVE_WITH_KNOTS ( 'NONE', 3,
 ( #12598, #13661, #7924, #5714, #4786, #11509 ),
 .UNSPECIFIED., .F., .F.,
 ( 4, 2, 4 ),
 ( 0.002950759650825690496, 0.004429055062152287107, 0.005907350473478885020 ),
 .UNSPECIFIED. ) ;
#6981 = EDGE_CURVE ( 'NONE', #8941, #8333, #10134, .T. ) ;
#6982 = VERTEX_POINT ( 'NONE', #4530 ) ;
#6983 = CARTESIAN_POINT ( 'NONE',  ( 0.03027795055833474094, 0.6888063905328563052, -3.499999999999995559 ) ) ;
#6984 = AXIS2_PLACEMENT_3D ( 'NONE', #9582, #5110, #1898 ) ;
#6985 = B_SPLINE_CURVE_WITH_KNOTS ( 'NONE', 3,
 ( #10736, #5173, #7133, #419 ),
 .UNSPECIFIED., .F., .F.,
 ( 4, 4 ),
 ( 0.002080789711329283660, 0.004173039763574516899 ),
 .UNSPECIFIED. ) ;
#6986 = CARTESIAN_POINT ( 'NONE',  ( 0.000000000000000000, 0.000000000000000000, 25.00000000000000000 ) ) ;
#6987 = DIRECTION ( 'NONE',  ( 0.000000000000000000, 0.000000000000000000, -1.000000000000000000 ) ) ;
#6988 = DIRECTION ( 'NONE',  ( 0.000000000000000000, 0.000000000000000000, -1.000000000000000000 ) ) ;
#6989 = EDGE_CURVE ( 'NONE', #696, #7740, #6763, .T. ) ;
#6990 = CARTESIAN_POINT ( 'NONE',  ( 21.68170757442799967, 141.2731697022880155, -32.99999999999999289 ) ) ;
#6991 = FACE_OUTER_BOUND ( 'NONE', #13888, .T. ) ;
#6992 = CARTESIAN_POINT ( 'NONE',  ( -3.081487911019577365E-30, 3.469446951953614189E-15, -6.000000000000005329 ) ) ;
#6993 = VECTOR ( 'NONE', #8395, 1000.000000000000000 ) ;
#6994 = VERTEX_POINT ( 'NONE', #12120 ) ;
#6995 =( BOUNDED_SURFACE ( )  B_SPLINE_SURFACE ( 3, 2, ( 
 ( #1493, #5935, #8578 ),
 ( #3046, #14162, #9750 ),
 ( #4144, #14303, #3115 ),
 ( #11890, #13209, #12997 ),
 ( #12098, #12921, #13067 ),
 ( #8727, #8515, #9691 ) ),
 .UNSPECIFIED., .F., .F., .F. ) 
 B_SPLINE_SURFACE_WITH_KNOTS ( ( 4, 2, 4 ),
 ( 3, 3 ),
 ( 0.01886329300151613764, 0.02121559706996257316, 0.02356790113840900522 ),
 ( 0.000000000000000000, 1.000000000000000000 ),
 .UNSPECIFIED. ) 
 GEOMETRIC_REPRESENTATION_ITEM ( )  RATIONAL_B_SPLINE_SURFACE ( (
 ( 1.000000000000000000, 0.8047780979744990626, 1.000000000000000000),
 ( 1.000000000000000000, 0.8123789428413605851, 1.000000000000000000),
 ( 1.000000000000000000, 0.8190677778298707246, 1.000000000000000000),
 ( 1.000000000000000000, 0.8192346266087571216, 1.000000000000000000),
 ( 1.000000000000000000, 0.8126126851684565278, 1.000000000000000000),
 ( 1.000000000000000000, 0.8047712636103355743, 1.000000000000000000) ) ) 
 REPRESENTATION_ITEM ( '' )  SURFACE ( )  );
#6996 = ORIENTED_EDGE ( 'NONE', *, *, #9342, .T. ) ;
#6997 = VERTEX_POINT ( 'NONE', #11092 ) ;
#6998 = DIRECTION ( 'NONE',  ( 0.9701425001453319874, 0.2425356250363328858, 0.000000000000000000 ) ) ;
#6999 = ORIENTED_EDGE ( 'NONE', *, *, #10923, .T. ) ;
#7000 = EDGE_CURVE ( 'NONE', #641, #1738, #8963, .T. ) ;
#7001 = EDGE_LOOP ( 'NONE', ( #11447, #13485, #2315, #9106, #3342, #317 ) ) ;
#7002 = FACE_OUTER_BOUND ( 'NONE', #9276, .T. ) ;
#7003 = CARTESIAN_POINT ( 'NONE',  ( 71.80728622811317052, -17.99808865627608512, 28.00000000000000000 ) ) ;
#7004 = LINE ( 'NONE', #11404, #9610 ) ;
#7005 = VECTOR ( 'NONE', #5607, 1000.000000000000000 ) ;
#7006 = VECTOR ( 'NONE', #9708, 1000.000000000000000 ) ;
#7007 = DIRECTION ( 'NONE',  ( 0.000000000000000000, 0.000000000000000000, -1.000000000000000000 ) ) ;
#7008 = DIRECTION ( 'NONE',  ( 1.000000000000000000, -5.046468293750711996E-16, -1.680811587828860421E-31 ) ) ;
#7009 = CARTESIAN_POINT ( 'NONE',  ( 31.80000000000005045, 6.938893903907228378E-15, 2.775557561562891351E-14 ) ) ;
#7010 = ORIENTED_EDGE ( 'NONE', *, *, #2494, .F. ) ;
#7011 = CARTESIAN_POINT ( 'NONE',  ( 58.68170757442803165, 34.50422595846453078, -28.00000000000000000 ) ) ;
#7012 = ORIENTED_EDGE ( 'NONE', *, *, #8323, .T. ) ;
#7013 = VECTOR ( 'NONE', #7878, 1000.000000000000000 ) ;
#7014 = MECHANICAL_DESIGN_GEOMETRIC_PRESENTATION_REPRESENTATION (  '', ( #4704 ), #9367 ) ;
#7015 = EDGE_LOOP ( 'NONE', ( #8069, #5644, #4595, #4226 ) ) ;
#7016 = EDGE_CURVE ( 'NONE', #6548, #13561, #2785, .T. ) ;
#7017 = CIRCLE ( 'NONE', #734, 5.499999999999984013 ) ;
#7018 = CARTESIAN_POINT ( 'NONE',  ( 31.38313257588138683, 143.6985259526510674, -25.00000000000000000 ) ) ;
#7019 = FACE_OUTER_BOUND ( 'NONE', #9918, .T. ) ;
#7020 = B_SPLINE_CURVE_WITH_KNOTS ( 'NONE', 3,
 ( #7055, #6027, #3934, #9258, #6979 ),
 .UNSPECIFIED., .F., .F.,
 ( 4, 1, 4 ),
 ( 0.000000000000000000, 0.002309401076758506657, 0.004618802153517013315 ),
 .UNSPECIFIED. ) ;
#7021 = VECTOR ( 'NONE', #12647, 1000.000000000000000 ) ;
#7022 = ORIENTED_EDGE ( 'NONE', *, *, #6620, .T. ) ;
#7023 = VECTOR ( 'NONE', #4691, 1000.000000000000000 ) ;
#7024 = ORIENTED_EDGE ( 'NONE', *, *, #12977, .T. ) ;
#7025 = FACE_BOUND ( 'NONE', #6447, .T. ) ;
#7026 = FACE_OUTER_BOUND ( 'NONE', #5720, .T. ) ;
#7027 = ORIENTED_EDGE ( 'NONE', *, *, #5413, .T. ) ;
#7028 = DIRECTION ( 'NONE',  ( -0.000000000000000000, -0.000000000000000000, -1.000000000000000000 ) ) ;
#7029 = EDGE_CURVE ( 'NONE', #13862, #12928, #10140, .T. ) ;
#7030 = VECTOR ( 'NONE', #2434, 999.9999999999998863 ) ;
#7031 = CONICAL_SURFACE ( 'NONE', #750, 5.371010071662830399, 1.221730476396037268 ) ;
#7032 = EDGE_CURVE ( 'NONE', #5057, #3097, #11016, .T. ) ;
#7033 = PLANE ( 'NONE',  #3535 ) ;
#7034 = CARTESIAN_POINT ( 'NONE',  ( 4.151274195509659037, 2.039912954708745119, 3.533232880573488721 ) ) ;
#7035 = CARTESIAN_POINT ( 'NONE',  ( -5.253368672218636348, 3.033033817057773085, -4.659491423763650886 ) ) ;
#7036 = PLANE ( 'NONE',  #2457 ) ;
#7037 = CARTESIAN_POINT ( 'NONE',  ( 0.6806757771994083051, 5.380514348699340310, -4.138711833382858529 ) ) ;
#7038 = CARTESIAN_POINT ( 'NONE',  ( 49.47979101891770171, 52.38859998837343568, 25.00000000000000000 ) ) ;
#7039 = ADVANCED_FACE ( 'NONE', ( #8679 ), #5384, .T. ) ;
#7040 = EDGE_LOOP ( 'NONE', ( #6551, #12347 ) ) ;
#7041 = DIRECTION ( 'NONE',  ( 1.000000000000000000, 0.000000000000000000, -0.000000000000000000 ) ) ;
#7042 = ORIENTED_EDGE ( 'NONE', *, *, #3901, .F. ) ;
#7043 = CARTESIAN_POINT ( 'NONE',  ( -4.999999999999998224, -1.366094737331735587E-14, -3.920524600599843978 ) ) ;
#7044 = VECTOR ( 'NONE', #2979, 1000.000000000000000 ) ;
#7045 = CARTESIAN_POINT ( 'NONE',  ( -0.1756478951291627899, 4.720212513052423731, -3.169390900447838000 ) ) ;
#7046 = ORIENTED_EDGE ( 'NONE', *, *, #2680, .F. ) ;
#7047 = CARTESIAN_POINT ( 'NONE',  ( 4.942464816488298496, -2.653516201069525238, -3.403975121040109020 ) ) ;
#7048 = FACE_OUTER_BOUND ( 'NONE', #5698, .T. ) ;
#7049 = VERTEX_POINT ( 'NONE', #4458 ) ;
#7050 = DIRECTION ( 'NONE',  ( -0.8191520442889900222, -1.364162190357603728E-16, -0.5735764363510484909 ) ) ;
#7051 = ORIENTED_EDGE ( 'NONE', *, *, #8195, .T. ) ;
#7052 = EDGE_CURVE ( 'NONE', #10813, #2320, #12058, .T. ) ;
#7053 = EDGE_LOOP ( 'NONE', ( #8519, #9156, #13557, #8225, #9029, #8892, #737, #5008 ) ) ;
#7054 = CARTESIAN_POINT ( 'NONE',  ( -68.68170757442807428, 29.57655509336050415, -106.9999999999999858 ) ) ;
#7055 = CARTESIAN_POINT ( 'NONE',  ( -4.000000000000000000, -2.309401076758511806, -3.133295621305376422 ) ) ;
#7056 =( GEOMETRIC_REPRESENTATION_CONTEXT ( 3 ) GLOBAL_UNCERTAINTY_ASSIGNED_CONTEXT ( ( #9235 ) ) GLOBAL_UNIT_ASSIGNED_CONTEXT ( ( #11658, #9469, #1558 ) ) REPRESENTATION_CONTEXT ( 'NONE', 'WORKASPACE' ) );
#7057 = CARTESIAN_POINT ( 'NONE',  ( 3.349226789952655992, 2.685125164760735039, -0.2236248678334833151 ) ) ;
#7058 = VECTOR ( 'NONE', #2163, 1000.000000000000000 ) ;
#7059 = CIRCLE ( 'NONE', #1466, 2.100000000000000977 ) ;
#7060 = CARTESIAN_POINT ( 'NONE',  ( -3.081487911019577365E-30, 3.469446951953614189E-15, -4.900000000000015454 ) ) ;
#7061 = DIRECTION ( 'NONE',  ( -1.000000000000000000, 0.000000000000000000, 0.000000000000000000 ) ) ;
#7062 = PRESENTATION_STYLE_ASSIGNMENT (( #6036 ) ) ;
#7063 = CARTESIAN_POINT ( 'NONE',  ( 0.000000000000000000, 0.000000000000000000, 0.000000000000000000 ) ) ;
#7064 = CARTESIAN_POINT ( 'NONE',  ( 0.1217565302851075920, 3.710888496608915510, -0.5725525826504623828 ) ) ;
#7065 = CARTESIAN_POINT ( 'NONE',  ( 18.68170757442808849, 141.2731697022877313, 35.00000000000000000 ) ) ;
#7066 = LINE ( 'NONE', #11685, #8590 ) ;
#7067 = APPLICATION_CONTEXT ( 'automotive_design' ) ;
#7068 = VECTOR ( 'NONE', #2891, 1000.000000000000000 ) ;
#7069 = EDGE_LOOP ( 'NONE', ( #10727, #12418, #11155, #14032 ) ) ;
#7070 = EDGE_CURVE ( 'NONE', #6578, #13498, #6621, .T. ) ;
#7071 = DIRECTION ( 'NONE',  ( -0.000000000000000000, -8.482162385747133845E-47, 1.000000000000000000 ) ) ;
#7072 = EDGE_CURVE ( 'NONE', #10603, #2504, #10240, .T. ) ;
#7073 = VERTEX_POINT ( 'NONE', #2248 ) ;
#7074 = CARTESIAN_POINT ( 'NONE',  ( 57.35294117647057277, -1.411764705882362358, -23.00000000000000000 ) ) ;
#7075 = LINE ( 'NONE', #4686, #258 ) ;
#7076 = DIRECTION ( 'NONE',  ( -1.840274199520073302E-17, -0.5000000000000013323, -0.8660254037844379305 ) ) ;
#7077 = ADVANCED_FACE ( 'NONE', ( #996 ), #3423, .F. ) ;
#7078 = DIRECTION ( 'NONE',  ( -0.9701425001453318764, -0.2425356250363329969, 0.000000000000000000 ) ) ;
#7079 = CARTESIAN_POINT ( 'NONE',  ( 31.38313257588138683, 143.6985259526510390, -28.00000000000000000 ) ) ;
#7080 = CARTESIAN_POINT ( 'NONE',  ( 0.000000000000000000, 1.387778780781445676E-14, 3.499999999999982236 ) ) ;
#7081 =( NAMED_UNIT ( * ) SI_UNIT ( $, .STERADIAN. ) SOLID_ANGLE_UNIT ( ) );
#7082 = DIRECTION ( 'NONE',  ( 1.000000000000000000, 0.000000000000000000, 0.000000000000000000 ) ) ;
#7083 = CARTESIAN_POINT ( 'NONE',  ( 54.33050351964436686, 32.98574998546678927, 25.00000000000000000 ) ) ;
#7084 = CIRCLE ( 'NONE', #2910, 2.500000000000002220 ) ;
#7085 = EDGE_CURVE ( 'NONE', #568, #8261, #9441, .T. ) ;
#7086 = CARTESIAN_POINT ( 'NONE',  ( 105.6817075744280743, 59.57655509336061073, 25.00000000000000000 ) ) ;
#7087 = ORIENTED_EDGE ( 'NONE', *, *, #2501, .T. ) ;
#7088 = AXIS2_PLACEMENT_3D ( 'NONE', #10237, #8994, #4491 ) ;
#7089 = VERTEX_POINT ( 'NONE', #6469 ) ;
#7090 = ORIENTED_EDGE ( 'NONE', *, *, #2464, .T. ) ;
#7091 = VECTOR ( 'NONE', #906, 1000.000000000000000 ) ;
#7092 = CARTESIAN_POINT ( 'NONE',  ( 108.6817075744280459, 189.5765550933606107, -106.9999999999999858 ) ) ;
#7093 = DIRECTION ( 'NONE',  ( 0.000000000000000000, 0.000000000000000000, -1.000000000000000000 ) ) ;
#7094 =( NAMED_UNIT ( * ) PLANE_ANGLE_UNIT ( ) SI_UNIT ( $, .RADIAN. ) );
#7095 = ORIENTED_EDGE ( 'NONE', *, *, #14443, .F. ) ;
#7096 = ORIENTED_EDGE ( 'NONE', *, *, #12732, .F. ) ;
#7097 = ORIENTED_EDGE ( 'NONE', *, *, #3707, .F. ) ;
#7098 = DIRECTION ( 'NONE',  ( -1.734723475976586383E-18, -0.4999999999999990008, 0.8660254037844391517 ) ) ;
#7099 = EDGE_CURVE ( 'NONE', #7193, #9446, #3227, .T. ) ;
#7100 = DIRECTION ( 'NONE',  ( 0.000000000000000000, 0.000000000000000000, 1.000000000000000000 ) ) ;
#7101 = ORIENTED_EDGE ( 'NONE', *, *, #3923, .F. ) ;
#7102 = CARTESIAN_POINT ( 'NONE',  ( 44.62907851819101523, 71.79144999128007498, 25.00000000000000000 ) ) ;
#7103 = EDGE_CURVE ( 'NONE', #4966, #1320, #2310, .T. ) ;
#7104 = ORIENTED_EDGE ( 'NONE', *, *, #12875, .F. ) ;
#7105 = DIRECTION ( 'NONE',  ( -0.000000000000000000, 1.000000000000000000, -0.000000000000000000 ) ) ;
#7106 = CARTESIAN_POINT ( 'NONE',  ( 54.35294117647056567, -1.411764705882362358, -25.00000000000000000 ) ) ;
#7107 = ORIENTED_EDGE ( 'NONE', *, *, #7274, .F. ) ;
#7108 = DIRECTION ( 'NONE',  ( 1.000000000000000000, 0.000000000000000000, 0.000000000000000000 ) ) ;
#7109 = CARTESIAN_POINT ( 'NONE',  ( 108.6817075744280743, 59.57655509336061073, 25.00000000000000000 ) ) ;
#7110 = SURFACE_SIDE_STYLE ('',( #1717 ) ) ;
#7111 = CYLINDRICAL_SURFACE ( 'NONE', #6931, 2.100000000000000977 ) ;
#7112 = DIRECTION ( 'NONE',  ( 1.000000000000000000, 1.224646799147353454E-16, 0.000000000000000000 ) ) ;
#7113 = EDGE_LOOP ( 'NONE', ( #7218, #7909, #158, #8950 ) ) ;
#7114 = CARTESIAN_POINT ( 'NONE',  ( 46.97979101891770171, 52.38859998837343568, 25.00000000000000000 ) ) ;
#7115 = CARTESIAN_POINT ( 'NONE',  ( 3.822382184081044798, 10.25936179483148969, 8.000000000000007105 ) ) ;
#7116 = ADVANCED_FACE ( 'NONE', ( #7573 ), #12055, .T. ) ;
#7117 = PRODUCT_RELATED_PRODUCT_CATEGORY ( 'part', '', ( #10587 ) ) ;
#7118 = CARTESIAN_POINT ( 'NONE',  ( -0.1410420225375824677, 4.700232803196133347, -3.387027626239151434 ) ) ;
#7119 = ORIENTED_EDGE ( 'NONE', *, *, #6298, .F. ) ;
#7120 = CARTESIAN_POINT ( 'NONE',  ( 4.966167347451191816, -2.723760149935152253, -3.431994069539848535 ) ) ;
#7121 = FACE_OUTER_BOUND ( 'NONE', #7956, .T. ) ;
#7122 = VERTEX_POINT ( 'NONE', #9853 ) ;
#7123 = DIRECTION ( 'NONE',  ( 0.000000000000000000, -6.695352868347746904E-17, 1.000000000000000000 ) ) ;
#7124 = ORIENTED_EDGE ( 'NONE', *, *, #10976, .F. ) ;
#7125 = ADVANCED_FACE ( 'NONE', ( #8751 ), #13805, .F. ) ;
#7126 = VERTEX_POINT ( 'NONE', #2677 ) ;
#7127 = DIRECTION ( 'NONE',  ( 0.000000000000000000, 0.000000000000000000, 1.000000000000000000 ) ) ;
#7128 = CARTESIAN_POINT ( 'NONE',  ( 58.68170757442803165, 29.57655509336062849, -33.00000000000000000 ) ) ;
#7129 = ORIENTED_EDGE ( 'NONE', *, *, #796, .F. ) ;
#7130 = PLANE ( 'NONE',  #9593 ) ;
#7131 = DIRECTION ( 'NONE',  ( -2.081668171172169499E-16, 0.000000000000000000, 1.000000000000000000 ) ) ;
#7132 =( LENGTH_UNIT ( ) NAMED_UNIT ( * ) SI_UNIT ( .MILLI., .METRE. ) );
#7133 = CARTESIAN_POINT ( 'NONE',  ( 4.050480423730761004, 1.376911654797406737, -3.567926555162020730 ) ) ;
#7134 = FILL_AREA_STYLE ('',( #10515 ) ) ;
#7135 = CONTEXT_DEPENDENT_SHAPE_REPRESENTATION ( #9226, #13429 ) ;
#7136 = CARTESIAN_POINT ( 'NONE',  ( -33.49999999999998579, 29.99999999999999645, 0.000000000000000000 ) ) ;
#7137 = CARTESIAN_POINT ( 'NONE',  ( -3.999999999999991118, -0.8232522521399826543, -3.130632262998142235 ) ) ;
#7138 = CARTESIAN_POINT ( 'NONE',  ( 53.99999999999997868, -1.347111479062091166E-15, 25.00000000000000000 ) ) ;
#7139 = LINE ( 'NONE', #6807, #1837 ) ;
#7140 = DIRECTION ( 'NONE',  ( -1.000000000000000000, 0.000000000000000000, 0.000000000000000000 ) ) ;
#7141 = ORIENTED_EDGE ( 'NONE', *, *, #7659, .F. ) ;
#7142 = ORIENTED_EDGE ( 'NONE', *, *, #9080, .F. ) ;
#7143 = FACE_BOUND ( 'NONE', #1572, .T. ) ;
#7144 = CARTESIAN_POINT ( 'NONE',  ( -2.750000000000003997, 40.49999999999999289, 8.000000000000007105 ) ) ;
#7145 = CARTESIAN_POINT ( 'NONE',  ( -24.99999999999998934, 189.5765550933606107, -2.000000000000001776 ) ) ;
#7146 = PLANE ( 'NONE',  #5127 ) ;
#7147 = CARTESIAN_POINT ( 'NONE',  ( 5.098157279263968000, -2.347014727359302722, -4.065148753898760958 ) ) ;
#7148 = CIRCLE ( 'NONE', #9512, 2.500000000000002220 ) ;
#7149 = DIRECTION ( 'NONE',  ( 0.000000000000000000, 0.000000000000000000, -1.000000000000000000 ) ) ;
#7150 = DIRECTION ( 'NONE',  ( -1.000000000000000000, 0.000000000000000000, 0.000000000000000000 ) ) ;
#7151 = DIRECTION ( 'NONE',  ( 1.000000000000000000, 0.000000000000000000, 0.000000000000000000 ) ) ;
#7152 = CARTESIAN_POINT ( 'NONE',  ( 129.3408537872138595, 199.5765550933606107, -80.00000000000002842 ) ) ;
#7153 = EDGE_CURVE ( 'NONE', #192, #3729, #4593, .T. ) ;
#7154 = CARTESIAN_POINT ( 'NONE',  ( 30.60000000000000853, 29.99999999999999645, -34.50000000000000000 ) ) ;
#7155 = VERTEX_POINT ( 'NONE', #1420 ) ;
#7156 = EDGE_CURVE ( 'NONE', #6805, #5852, #11869, .T. ) ;
#7157 = ORIENTED_EDGE ( 'NONE', *, *, #12024, .T. ) ;
#7158 = VECTOR ( 'NONE', #10284, 1000.000000000000000 ) ;
#7159 = CARTESIAN_POINT ( 'NONE',  ( 20.00000000000000355, 50.00000000000000000, -25.00000000000000000 ) ) ;
#7160 = CARTESIAN_POINT ( 'NONE',  ( -6.532899837730830939, 4.269496439496346535E-15, -5.432899837730820636 ) ) ;
#7161 = EDGE_CURVE ( 'NONE', #13574, #4466, #8140, .T. ) ;
#7162 = ORIENTED_EDGE ( 'NONE', *, *, #2244, .T. ) ;
#7163 = EDGE_CURVE ( 'NONE', #11932, #5040, #11517, .T. ) ;
#7164 = VERTEX_POINT ( 'NONE', #5865 ) ;
#7165 = AXIS2_PLACEMENT_3D ( 'NONE', #13591, #10198, #184 ) ;
#7166 = CARTESIAN_POINT ( 'NONE',  ( 5.170224855064536662, -2.788471980053871757, -4.589066185948674104 ) ) ;
#7167 = AXIS2_PLACEMENT_3D ( 'NONE', #2774, #7214, #3943 ) ;
#7168 = LINE ( 'NONE', #10251, #5420 ) ;
#7169 = EDGE_LOOP ( 'NONE', ( #6695, #2871 ) ) ;
#7170 = B_SPLINE_CURVE_WITH_KNOTS ( 'NONE', 3,
 ( #12046, #783, #7357, #11832, #6255, #10730, #14390, #10056, #11220, #10189 ),
 .UNSPECIFIED., .F., .F.,
 ( 4, 2, 2, 2, 4 ),
 ( 0.000000000000000000, 0.001528561485809836482, 0.003057122971619672964, 0.004585684457429509663, 0.006114245943239347662 ),
 .UNSPECIFIED. ) ;
#7171 = DIRECTION ( 'NONE',  ( -0.2425356250363330801, 0.9701425001453319874, 0.000000000000000000 ) ) ;
#7172 = PRODUCT_DEFINITION_SHAPE ( 'NONE', 'NONE',  #14469 ) ;
#7173 = B_SPLINE_CURVE_WITH_KNOTS ( 'NONE', 3,
 ( #14382, #8867, #9979, #7616, #2157 ),
 .UNSPECIFIED., .F., .F.,
 ( 4, 1, 4 ),
 ( 0.000000000000000000, 0.002886751345948135056, 0.005773502691896270113 ),
 .UNSPECIFIED. ) ;
#7174 = UNCERTAINTY_MEASURE_WITH_UNIT (LENGTH_MEASURE( 1.000000000000000082E-05 ), #1276, 'distance_accuracy_value', 'NONE');
#7175 = DIRECTION ( 'NONE',  ( -1.000000000000000000, -1.665334536937734071E-16, -0.000000000000000000 ) ) ;
#7176 = CARTESIAN_POINT ( 'NONE',  ( 4.124214193018063135, 2.028338413290930120, 3.513185186763549073 ) ) ;
#7177 = DIRECTION ( 'NONE',  ( -1.000000000000000000, 0.000000000000000000, 0.000000000000000000 ) ) ;
#7178 = AXIS2_PLACEMENT_3D ( 'NONE', #10598, #11611, #10520 ) ;
#7179 = EDGE_CURVE ( 'NONE', #13364, #14315, #8730, .T. ) ;
#7180 = VECTOR ( 'NONE', #7565, 1000.000000000000000 ) ;
#7181 = VECTOR ( 'NONE', #4543, 1000.000000000000000 ) ;
#7182 = CARTESIAN_POINT ( 'NONE',  ( 22.00000000000000000, 70.00000000000000000, -25.00000000000000000 ) ) ;
#7183 = FACE_BOUND ( 'NONE', #10459, .T. ) ;
#7184 = ORIENTED_EDGE ( 'NONE', *, *, #7427, .T. ) ;
#7185 = DIRECTION ( 'NONE',  ( -1.000000000000000000, -3.286707217423839940E-17, -2.273843122241288053E-18 ) ) ;
#7186 = CARTESIAN_POINT ( 'NONE',  ( 28.00000000000000355, 35.49999999999997868, 8.000000000000007105 ) ) ;
#7187 = ORIENTED_EDGE ( 'NONE', *, *, #7762, .F. ) ;
#7188 = CARTESIAN_POINT ( 'NONE',  ( 28.00000000000000355, 29.99999999999999645, -25.00000000000000000 ) ) ;
#7189 = VERTEX_POINT ( 'NONE', #11441 ) ;
#7190 = LINE ( 'NONE', #4934, #10247 ) ;
#7191 = EDGE_CURVE ( 'NONE', #11970, #4249, #13051, .T. ) ;
#7192 = CARTESIAN_POINT ( 'NONE',  ( 0.6810530063608244422, 4.461079733297845351, -3.298443181296111248 ) ) ;
#7193 = VERTEX_POINT ( 'NONE', #401 ) ;
#7194 = CARTESIAN_POINT ( 'NONE',  ( 0.6937372685066715006, -4.453844082567738560, -3.310536846335876859 ) ) ;
#7195 = B_SPLINE_CURVE_WITH_KNOTS ( 'NONE', 3,
 ( #493, #9183, #3791, #7057, #1578, #13680 ),
 .UNSPECIFIED., .F., .F.,
 ( 4, 2, 4 ),
 ( 0.002365888236227995517, 0.003551327329835083681, 0.004736766423442171844 ),
 .UNSPECIFIED. ) ;
#7196 = AXIS2_PLACEMENT_3D ( 'NONE', #6470, #5252, #14258 ) ;
#7197 = CARTESIAN_POINT ( 'NONE',  ( 20.00000000000000000, 37.00000000000000711, -25.00000000000000000 ) ) ;
#7198 = CIRCLE ( 'NONE', #4865, 2.750000000000003553 ) ;
#7199 = B_SPLINE_CURVE_WITH_KNOTS ( 'NONE', 3,
 ( #11055, #8850, #948, #2133, #10024 ),
 .UNSPECIFIED., .F., .F.,
 ( 4, 1, 4 ),
 ( 0.000000000000000000, 0.002309401076758505790, 0.004618802153517011580 ),
 .UNSPECIFIED. ) ;
#7200 = DIRECTION ( 'NONE',  ( 0.000000000000000000, 0.000000000000000000, 1.000000000000000000 ) ) ;
#7201 = VERTEX_POINT ( 'NONE', #333 ) ;
#7202 = ORIENTED_EDGE ( 'NONE', *, *, #3686, .F. ) ;
#7203 = DIRECTION ( 'NONE',  ( 0.000000000000000000, 0.000000000000000000, -1.000000000000000000 ) ) ;
#7204 = DIRECTION ( 'NONE',  ( 0.000000000000000000, 0.000000000000000000, -1.000000000000000000 ) ) ;
#7205 = EDGE_CURVE ( 'NONE', #11468, #12380, #10697, .T. ) ;
#7206 = ORIENTED_EDGE ( 'NONE', *, *, #1040, .T. ) ;
#7207 = CARTESIAN_POINT ( 'NONE',  ( 4.082498951862936210, -4.041451884327377009, 2.512980736065759382E-20 ) ) ;
#7208 = EDGE_CURVE ( 'NONE', #32, #14260, #13987, .T. ) ;
#7209 = LINE ( 'NONE', #494, #7630 ) ;
#7210 = CARTESIAN_POINT ( 'NONE',  ( -24.99999999999999289, 189.5765550933606107, 47.99999999999998579 ) ) ;
#7211 = VECTOR ( 'NONE', #2767, 1000.000000000000000 ) ;
#7212 = PRESENTATION_STYLE_ASSIGNMENT (( #496 ) ) ;
#7213 = CARTESIAN_POINT ( 'NONE',  ( 5.551115123125782702E-14, -3.464101615137743728, 2.000000000000001776 ) ) ;
#7214 = DIRECTION ( 'NONE',  ( 0.000000000000000000, 0.000000000000000000, -1.000000000000000000 ) ) ;
#7215 = LINE ( 'NONE', #5034, #9866 ) ;
#7216 = DIRECTION ( 'NONE',  ( 0.000000000000000000, 0.000000000000000000, 1.000000000000000000 ) ) ;
#7217 = ORIENTED_EDGE ( 'NONE', *, *, #2543, .F. ) ;
#7218 = ORIENTED_EDGE ( 'NONE', *, *, #7698, .T. ) ;
#7219 = CARTESIAN_POINT ( 'NONE',  ( 4.000000000000004441, -0.3979232138631220717, -4.518073740654438009E-15 ) ) ;
#7220 = EDGE_LOOP ( 'NONE', ( #2210, #14387 ) ) ;
#7221 = ORIENTED_EDGE ( 'NONE', *, *, #6968, .T. ) ;
#7222 = DIRECTION ( 'NONE',  ( -1.000000000000000000, 0.000000000000000000, 0.000000000000000000 ) ) ;
#7223 = AXIS2_PLACEMENT_3D ( 'NONE', #6418, #12131, #4178 ) ;
#7224 = CARTESIAN_POINT ( 'NONE',  ( 56.83050351964436686, 32.98574998546678927, 25.00000000000000000 ) ) ;
#7225 = CARTESIAN_POINT ( 'NONE',  ( -28.00000000000000355, 29.99999999999999645, 8.000000000000007105 ) ) ;
#7226 = DIRECTION ( 'NONE',  ( 0.8660254037844373753, 0.5000000000000022204, 2.348866325434637045E-33 ) ) ;
#7227 = DIRECTION ( 'NONE',  ( 0.000000000000000000, 0.000000000000000000, -1.000000000000000000 ) ) ;
#7228 = CARTESIAN_POINT ( 'NONE',  ( 79.68170757442804586, 124.5765550933606249, 25.00000000000000000 ) ) ;
#7229 = CARTESIAN_POINT ( 'NONE',  ( 28.00000000000000355, 29.99999999999999645, -40.12500000000000000 ) ) ;
#7230 = FACE_OUTER_BOUND ( 'NONE', #12906, .T. ) ;
#7231 = CARTESIAN_POINT ( 'NONE',  ( 2.749999999999997780, 25.49999999999996803, 8.000000000000007105 ) ) ;
#7232 = EDGE_CURVE ( 'NONE', #7417, #12192, #5942, .T. ) ;
#7233 = CARTESIAN_POINT ( 'NONE',  ( 20.00000000000000000, 5.000000000000000000, -25.00000000000000000 ) ) ;
#7234 = ORIENTED_EDGE ( 'NONE', *, *, #3611, .T. ) ;
#7235 = VERTEX_POINT ( 'NONE', #3773 ) ;
#7236 = VERTEX_POINT ( 'NONE', #8216 ) ;
#7237 = EDGE_CURVE ( 'NONE', #36, #11314, #12687, .T. ) ;
#7238 = CIRCLE ( 'NONE', #2580, 5.000000000000000888 ) ;
#7239 = EDGE_CURVE ( 'NONE', #1551, #10480, #4850, .T. ) ;
#7240 = PLANE ( 'NONE',  #2883 ) ;
#7241 = DIRECTION ( 'NONE',  ( 1.000000000000000000, 0.000000000000000000, 0.000000000000000000 ) ) ;
#7242 = EDGE_CURVE ( 'NONE', #2779, #11645, #6505, .T. ) ;
#7243 = DIRECTION ( 'NONE',  ( 0.000000000000000000, 0.000000000000000000, -1.000000000000000000 ) ) ;
#7244 = VECTOR ( 'NONE', #2054, 1000.000000000000000 ) ;
#7245 = VECTOR ( 'NONE', #13826, 1000.000000000000000 ) ;
#7246 = CARTESIAN_POINT ( 'NONE',  ( -1.598077599629839529, -4.850852159564174038, -4.271474537231504165 ) ) ;
#7247 = ORIENTED_EDGE ( 'NONE', *, *, #13289, .T. ) ;
#7248 = ADVANCED_FACE ( 'NONE', ( #257 ), #5721, .T. ) ;
#7249 = CARTESIAN_POINT ( 'NONE',  ( 33.99999999999998579, 80.00000000000000000, 25.00000000000000000 ) ) ;
#7250 = ORIENTED_EDGE ( 'NONE', *, *, #10086, .T. ) ;
#7251 = VECTOR ( 'NONE', #9922, 1000.000000000000000 ) ;
#7252 = EDGE_CURVE ( 'NONE', #10823, #3711, #9172, .T. ) ;
#7253 = CARTESIAN_POINT ( 'NONE',  ( 5.551115123125782702E-14, 1.387778780781445676E-14, -4.000000000000003553 ) ) ;
#7254 = CARTESIAN_POINT ( 'NONE',  ( 30.10000000000000497, 29.99999999999999645, -6.999999999999992006 ) ) ;
#7255 = FACE_OUTER_BOUND ( 'NONE', #6972, .T. ) ;
#7256 = ADVANCED_FACE ( 'NONE', ( #3633 ), #8067, .T. ) ;
#7257 = ORIENTED_EDGE ( 'NONE', *, *, #2805, .F. ) ;
#7258 = VECTOR ( 'NONE', #6132, 1000.000000000000000 ) ;
#7259 = CARTESIAN_POINT ( 'NONE',  ( 4.165266963751704132, 4.099263933823992012, -1.430665712853978865E-14 ) ) ;
#7260 = AXIS2_PLACEMENT_3D ( 'NONE', #7188, #11895, #12927 ) ;
#7261 = PLANE ( 'NONE',  #138 ) ;
#7262 = ORIENTED_EDGE ( 'NONE', *, *, #12274, .F. ) ;
#7263 = CARTESIAN_POINT ( 'NONE',  ( 40.00000000000000711, 80.00000000000000000, -25.00000000000000000 ) ) ;
#7264 =( REPRESENTATION_RELATIONSHIP ('NONE','NONE', #10295, #1400 ) REPRESENTATION_RELATIONSHIP_WITH_TRANSFORMATION ( #12557 )SHAPE_REPRESENTATION_RELATIONSHIP( ) );
#7265 = CARTESIAN_POINT ( 'NONE',  ( -6.726859516510133474, 3.469446951953614189E-15, -4.900000000000015454 ) ) ;
#7266 = CIRCLE ( 'NONE', #957, 4.600000000000003197 ) ;
#7267 = ORIENTED_EDGE ( 'NONE', *, *, #7085, .F. ) ;
#7268 = DIRECTION ( 'NONE',  ( 0.3420201433256625512, -4.092221844761578132E-17, -0.9396926207859105373 ) ) ;
#7269 = ORIENTED_EDGE ( 'NONE', *, *, #5285, .F. ) ;
#7270 = CARTESIAN_POINT ( 'NONE',  ( -13.00000000000000533, 24.50000000000001421, 8.000000000000007105 ) ) ;
#7271 = CARTESIAN_POINT ( 'NONE',  ( 2.756166666307359847, 3.027528586792976650, -2.923144239647418541 ) ) ;
#7272 = VERTEX_POINT ( 'NONE', #11966 ) ;
#7273 = DIRECTION ( 'NONE',  ( 1.000000000000000000, 2.133709875451472726E-16, 0.000000000000000000 ) ) ;
#7274 = EDGE_CURVE ( 'NONE', #13002, #2748, #2083, .T. ) ;
#7275 = CIRCLE ( 'NONE', #5853, 1.500000000000000000 ) ;
#7276 = CARTESIAN_POINT ( 'NONE',  ( -3.999999999999996447, 2.309401076758494487, -3.133295621305376422 ) ) ;
#7277 = AXIS2_PLACEMENT_3D ( 'NONE', #864, #5117, #5193 ) ;
#7278 = DIRECTION ( 'NONE',  ( -0.000000000000000000, 1.000000000000000000, 0.000000000000000000 ) ) ;
#7279 = ORIENTED_EDGE ( 'NONE', *, *, #10501, .F. ) ;
#7280 = ORIENTED_EDGE ( 'NONE', *, *, #11548, .F. ) ;
#7281 = LINE ( 'NONE', #9407, #5684 ) ;
#7282 = CARTESIAN_POINT ( 'NONE',  ( 3.000000000000000888, 3.836840991697820422E-15, -5.974599999999997024 ) ) ;
#7283 = EDGE_CURVE ( 'NONE', #1772, #12392, #6246, .T. ) ;
#7284 = ORIENTED_EDGE ( 'NONE', *, *, #12458, .T. ) ;
#7285 = CARTESIAN_POINT ( 'NONE',  ( 4.175326769692884632, -4.121399112977863766, 1.938140992669738524E-14 ) ) ;
#7286 = DIRECTION ( 'NONE',  ( -2.133709875451472726E-16, 1.000000000000000000, 0.000000000000000000 ) ) ;
#7287 = AXIS2_PLACEMENT_3D ( 'NONE', #1433, #5800, #7204 ) ;
#7288 = SURFACE_SIDE_STYLE ('',( #10735 ) ) ;
#7289 = VECTOR ( 'NONE', #9830, 1000.000000000000000 ) ;
#7290 = FACE_BOUND ( 'NONE', #9103, .T. ) ;
#7291 = CIRCLE ( 'NONE', #8218, 5.000000000000000888 ) ;
#7292 = AXIS2_PLACEMENT_3D ( 'NONE', #10920, #6241, #6521 ) ;
#7293 = ORIENTED_EDGE ( 'NONE', *, *, #580, .F. ) ;
#7294 = CARTESIAN_POINT ( 'NONE',  ( 108.6817075744280174, 69.57655509336049704, 1.592040838891559450E-14 ) ) ;
#7295 = DIRECTION ( 'NONE',  ( 0.000000000000000000, 1.224646799147353207E-16, -1.000000000000000000 ) ) ;
#7296 = FACE_OUTER_BOUND ( 'NONE', #2648, .T. ) ;
#7297 = CARTESIAN_POINT ( 'NONE',  ( 28.00000000000000355, 29.99999999999999645, -34.50000000000000000 ) ) ;
#7298 = EDGE_CURVE ( 'NONE', #10355, #13672, #7190, .T. ) ;
#7299 = ORIENTED_EDGE ( 'NONE', *, *, #9678, .T. ) ;
#7300 = CIRCLE ( 'NONE', #6592, 2.000000000000001776 ) ;
#7301 = ORIENTED_EDGE ( 'NONE', *, *, #3852, .T. ) ;
#7302 = DIRECTION ( 'NONE',  ( -0.000000000000000000, -0.000000000000000000, -1.000000000000000000 ) ) ;
#7303 = ORIENTED_EDGE ( 'NONE', *, *, #5600, .T. ) ;
#7304 = ORIENTED_EDGE ( 'NONE', *, *, #12918, .F. ) ;
#7305 = FACE_OUTER_BOUND ( 'NONE', #5941, .T. ) ;
#7306 = DIRECTION ( 'NONE',  ( -1.000000000000000000, -1.723842398015259277E-15, 0.000000000000000000 ) ) ;
#7307 = DIRECTION ( 'NONE',  ( 1.000000000000000000, 0.000000000000000000, 0.000000000000000000 ) ) ;
#7308 = CARTESIAN_POINT ( 'NONE',  ( 5.099999999999993427, 2.886579864025407597E-16, 5.200000000000001066 ) ) ;
#7309 = VERTEX_POINT ( 'NONE', #10720 ) ;
#7310 = PLANE ( 'NONE',  #8448 ) ;
#7311 = PRODUCT_CONTEXT ( 'NONE', #5574, 'mechanical' ) ;
#7312 = CYLINDRICAL_SURFACE ( 'NONE', #10558, 2.749999999999997780 ) ;
#7313 = DIRECTION ( 'NONE',  ( 1.987661601597216239E-18, 4.440892098500621724E-16, 1.000000000000000000 ) ) ;
#7314 = AXIS2_PLACEMENT_3D ( 'NONE', #12938, #9761, #14240 ) ;
#7315 = ORIENTED_EDGE ( 'NONE', *, *, #5733, .F. ) ;
#7316 = EDGE_CURVE ( 'NONE', #181, #2621, #8444, .T. ) ;
#7317 = PRODUCT_RELATED_PRODUCT_CATEGORY ( 'part', '', ( #1709 ) ) ;
#7318 = EDGE_CURVE ( 'NONE', #14168, #12241, #2978, .T. ) ;
#7319 = DIRECTION ( 'NONE',  ( 0.000000000000000000, 0.000000000000000000, 1.000000000000000000 ) ) ;
#7320 = ORIENTED_EDGE ( 'NONE', *, *, #7191, .T. ) ;
#7321 = EDGE_LOOP ( 'NONE', ( #2598, #7918, #13930, #3894 ) ) ;
#7322 = AXIS2_PLACEMENT_3D ( 'NONE', #2811, #9157, #13653 ) ;
#7323 = CARTESIAN_POINT ( 'NONE',  ( 20.00000000000000355, 30.00000000000000711, -25.00000000000000000 ) ) ;
#7324 = CARTESIAN_POINT ( 'NONE',  ( 0.2182387239031207404, 1.693823289467343063, 3.499999999999995559 ) ) ;
#7325 = ORIENTED_EDGE ( 'NONE', *, *, #3655, .F. ) ;
#7326 = PRODUCT_DEFINITION_FORMATION_WITH_SPECIFIED_SOURCE ( 'ANY', '', #12672, .NOT_KNOWN. ) ;
#7327 = CARTESIAN_POINT ( 'NONE',  ( 21.68170757442808849, 141.2731697022877313, 25.00000000000000000 ) ) ;
#7328 = CARTESIAN_POINT ( 'NONE',  ( -1.582370436564039196, -4.859920694388334184, -4.019399823476004663 ) ) ;
#7329 = VERTEX_POINT ( 'NONE', #8585 ) ;
#7330 = FACE_OUTER_BOUND ( 'NONE', #4017, .T. ) ;
#7331 = AXIS2_PLACEMENT_3D ( 'NONE', #9488, #8226, #1736 ) ;
#7332 = UNCERTAINTY_MEASURE_WITH_UNIT (LENGTH_MEASURE( 1.000000000000000082E-05 ), #2288, 'distance_accuracy_value', 'NONE');
#7333 = CARTESIAN_POINT ( 'NONE',  ( 3.999999999999993339, -5.421010862427522170E-15, -2.842992957459210324 ) ) ;
#7334 = CARTESIAN_POINT ( 'NONE',  ( 0.1388410611046067000, -3.710337782248029015, -0.5735064479039794216 ) ) ;
#7335 = CARTESIAN_POINT ( 'NONE',  ( 0.2486750293982121773, -1.933232340707288888, 4.000000000000003553 ) ) ;
#7336 = ORIENTED_EDGE ( 'NONE', *, *, #10244, .T. ) ;
#7337 = DIRECTION ( 'NONE',  ( 0.000000000000000000, 8.482162385747133845E-47, -1.000000000000000000 ) ) ;
#7338 = CARTESIAN_POINT ( 'NONE',  ( 0.000000000000000000, 0.000000000000000000, 33.00000000000002842 ) ) ;
#7339 = ORIENTED_EDGE ( 'NONE', *, *, #4727, .F. ) ;
#7340 = CARTESIAN_POINT ( 'NONE',  ( 4.962664318264807584, 2.733102959025825562, -3.415681285064340766 ) ) ;
#7341 = ORIENTED_EDGE ( 'NONE', *, *, #11807, .F. ) ;
#7342 = DIRECTION ( 'NONE',  ( 0.000000000000000000, -0.000000000000000000, -1.000000000000000000 ) ) ;
#7343 = ORIENTED_EDGE ( 'NONE', *, *, #3550, .T. ) ;
#7344 = FACE_OUTER_BOUND ( 'NONE', #4832, .T. ) ;
#7345 = VECTOR ( 'NONE', #5615, 1000.000000000000000 ) ;
#7346 = VERTEX_POINT ( 'NONE', #700 ) ;
#7347 = CARTESIAN_POINT ( 'NONE',  ( 40.00000000000000711, 80.00000000000000000, 25.00000000000000000 ) ) ;
#7348 = EDGE_CURVE ( 'NONE', #1645, #1073, #12761, .T. ) ;
#7349 = VERTEX_POINT ( 'NONE', #3921 ) ;
#7350 = CARTESIAN_POINT ( 'NONE',  ( 5.599999999999994316, 4.041451884327390331, 0.000000000000000000 ) ) ;
#7351 = ADVANCED_FACE ( 'NONE', ( #5157 ), #9619, .T. ) ;
#7352 = FACE_BOUND ( 'NONE', #6893, .T. ) ;
#7353 = CARTESIAN_POINT ( 'NONE',  ( 30.10000000000000497, 29.99999999999999645, -25.00000000000000000 ) ) ;
#7354 = ORIENTED_EDGE ( 'NONE', *, *, #6151, .T. ) ;
#7355 = EDGE_LOOP ( 'NONE', ( #1141, #7320, #2678, #4175 ) ) ;
#7356 = DIRECTION ( 'NONE',  ( 1.000000000000000000, -0.000000000000000000, -0.000000000000000000 ) ) ;
#7357 = CARTESIAN_POINT ( 'NONE',  ( -0.8665032349992132232, -5.555903485205178960, -4.490643565754968591 ) ) ;
#7358 = APPLICATION_CONTEXT ( 'automotive_design' ) ;
#7359 = ORIENTED_EDGE ( 'NONE', *, *, #6417, .T. ) ;
#7360 = CARTESIAN_POINT ( 'NONE',  ( 4.175075985190124683, -4.120741555260251765, 1.387778780781445676E-14 ) ) ;
#7361 = CARTESIAN_POINT ( 'NONE',  ( -25.00000000000000000, 189.5765550933606107, 47.99999999999998579 ) ) ;
#7362 = DIRECTION ( 'NONE',  ( 0.000000000000000000, -0.000000000000000000, -1.000000000000000000 ) ) ;
#7363 = ADVANCED_FACE ( 'NONE', ( #9396 ), #1941, .F. ) ;
#7364 = CARTESIAN_POINT ( 'NONE',  ( 3.973110223767151616, 2.262797354954571809E-11, 3.565797985667430225 ) ) ;
#7365 = ORIENTED_EDGE ( 'NONE', *, *, #5636, .T. ) ;
#7366 = PLANE ( 'NONE',  #6253 ) ;
#7367 = EDGE_CURVE ( 'NONE', #5200, #45, #11745, .T. ) ;
#7368 = CARTESIAN_POINT ( 'NONE',  ( 0.3198814748697595411, 4.434118497892185040, -0.3507732604232542406 ) ) ;
#7369 = ORIENTED_EDGE ( 'NONE', *, *, #6624, .F. ) ;
#7370 = ORIENTED_EDGE ( 'NONE', *, *, #11403, .T. ) ;
#7371 = DIRECTION ( 'NONE',  ( 0.000000000000000000, 0.000000000000000000, -1.000000000000000000 ) ) ;
#7372 = ORIENTED_EDGE ( 'NONE', *, *, #13842, .T. ) ;
#7373 = EDGE_LOOP ( 'NONE', ( #7452, #14388, #5180, #5516, #11667, #4592 ) ) ;
#7374 = PLANE ( 'NONE',  #3981 ) ;
#7375 = DIRECTION ( 'NONE',  ( 0.000000000000000000, 0.000000000000000000, 1.000000000000000000 ) ) ;
#7376 = DIRECTION ( 'NONE',  ( -1.000000000000000000, 0.000000000000000000, 0.000000000000000000 ) ) ;
#7377 = AXIS2_PLACEMENT_3D ( 'NONE', #3178, #9819, #1113 ) ;
#7378 = EDGE_CURVE ( 'NONE', #8822, #10603, #2752, .T. ) ;
#7379 = CARTESIAN_POINT ( 'NONE',  ( 61.68121602037100359, 13.58289998256015352, 25.00000000000000000 ) ) ;
#7380 = DIRECTION ( 'NONE',  ( -1.000000000000000000, 0.000000000000000000, 0.000000000000000000 ) ) ;
#7381 = APPLICATION_PROTOCOL_DEFINITION ( 'draft international standard', 'automotive_design', 1998, #10449 ) ;
#7382 = CARTESIAN_POINT ( 'NONE',  ( -4.211140560182194292, 2.431303136016534250, -3.445885042887453231 ) ) ;
#7383 = DIRECTION ( 'NONE',  ( -1.000000000000000000, 0.000000000000000000, 0.000000000000000000 ) ) ;
#7384 = ADVANCED_FACE ( 'NONE', ( #7409 ), #6178, .F. ) ;
#7385 = CARTESIAN_POINT ( 'NONE',  ( 2.176667689905607883, 4.790324513057876210, -4.357749648769117634 ) ) ;
#7386 = ORIENTED_EDGE ( 'NONE', *, *, #9049, .T. ) ;
#7387 = CARTESIAN_POINT ( 'NONE',  ( 44.55443476855437268, 62.09002498982675888, 25.00000000000000000 ) ) ;
#7388 = CARTESIAN_POINT ( 'NONE',  ( 62.10586122665986863, -20.42344490663941414, 28.00000000000000000 ) ) ;
#7389 = SHAPE_REPRESENTATION ( 'Guide Rail Channel Shoe', ( #11025 ), #758 ) ;
#7390 = EDGE_CURVE ( 'NONE', #12268, #10194, #13169, .T. ) ;
#7391 = EDGE_CURVE ( 'NONE', #1551, #3920, #10650, .T. ) ;
#7392 = ORIENTED_EDGE ( 'NONE', *, *, #5237, .F. ) ;
#7393 = CARTESIAN_POINT ( 'NONE',  ( -0.03111943836866669019, -6.084399642271201003, -4.666192694417985010 ) ) ;
#7394 = LINE ( 'NONE', #7458, #10339 ) ;
#7395 = VECTOR ( 'NONE', #9538, 1000.000000000000114 ) ;
#7396 = VERTEX_POINT ( 'NONE', #7270 ) ;
#7397 = DIRECTION ( 'NONE',  ( 0.000000000000000000, 0.4999999999999996669, 0.8660254037844388186 ) ) ;
#7398 = CARTESIAN_POINT ( 'NONE',  ( 60.00000000000000000, -6.123233995736768255E-16, 25.00000000000000000 ) ) ;
#7399 = DIRECTION ( 'NONE',  ( 0.000000000000000000, 0.000000000000000000, -1.000000000000000000 ) ) ;
#7400 = DIRECTION ( 'NONE',  ( -1.000000000000000000, 0.000000000000000000, 0.000000000000000000 ) ) ;
#7401 = ORIENTED_EDGE ( 'NONE', *, *, #7000, .F. ) ;
#7402 = CARTESIAN_POINT ( 'NONE',  ( -5.244800587397357106, -2.026986389275633016, -4.490560292650636498 ) ) ;
#7403 = DIRECTION ( 'NONE',  ( -0.9701425001453325425, -0.2425356250363304988, 0.000000000000000000 ) ) ;
#7404 = ORIENTED_EDGE ( 'NONE', *, *, #824, .T. ) ;
#7405 = FACE_OUTER_BOUND ( 'NONE', #13889, .T. ) ;
#7406 = AXIS2_PLACEMENT_3D ( 'NONE', #6395, #9760, #13151 ) ;
#7407 = ORIENTED_EDGE ( 'NONE', *, *, #5481, .T. ) ;
#7408 = ORIENTED_EDGE ( 'NONE', *, *, #4370, .F. ) ;
#7409 = FACE_OUTER_BOUND ( 'NONE', #14417, .T. ) ;
#7410 = DIRECTION ( 'NONE',  ( -0.9701425001453319874, -0.2425356250363328858, 0.000000000000000000 ) ) ;
#7411 = ORIENTED_EDGE ( 'NONE', *, *, #6384, .T. ) ;
#7412 = CARTESIAN_POINT ( 'NONE',  ( 2.500000000000002220, 4.163336342344338999E-16, -25.03750572909319061 ) ) ;
#7413 = PLANE ( 'NONE',  #6139 ) ;
#7414 = CIRCLE ( 'NONE', #9294, 4.750000000000000000 ) ;
#7415 = EDGE_LOOP ( 'NONE', ( #4026, #13852, #2798, #836, #4551, #11823, #8359 ) ) ;
#7416 = AXIS2_PLACEMENT_3D ( 'NONE', #10078, #12282, #5606 ) ;
#7417 = VERTEX_POINT ( 'NONE', #5231 ) ;
#7418 = CARTESIAN_POINT ( 'NONE',  ( 19.99999999999999645, 57.00000000000000000, -25.00000000000000000 ) ) ;
#7419 = CARTESIAN_POINT ( 'NONE',  ( -1.051966859446179292, 48.43488408057972805, 0.1316037626694079032 ) ) ;
#7420 = ORIENTED_EDGE ( 'NONE', *, *, #6865, .F. ) ;
#7421 = CARTESIAN_POINT ( 'NONE',  ( -28.00000000000000355, 29.99999999999999645, 8.000000000000007105 ) ) ;
#7422 = EDGE_CURVE ( 'NONE', #2703, #10163, #5076, .T. ) ;
#7423 = DIRECTION ( 'NONE',  ( -1.000000000000000000, 0.000000000000000000, 0.000000000000000000 ) ) ;
#7424 = CARTESIAN_POINT ( 'NONE',  ( 4.033906725095162571, -1.419670120618688136, 3.499999999999992895 ) ) ;
#7425 = ORIENTED_EDGE ( 'NONE', *, *, #8014, .T. ) ;
#7426 = PRESENTATION_STYLE_ASSIGNMENT (( #9639 ) ) ;
#7427 = EDGE_CURVE ( 'NONE', #5863, #13172, #12100, .T. ) ;
#7428 = AXIS2_PLACEMENT_3D ( 'NONE', #385, #1193, #3680 ) ;
#7429 = DIRECTION ( 'NONE',  ( 0.000000000000000000, 0.000000000000000000, -1.000000000000000000 ) ) ;
#7430 = AXIS2_PLACEMENT_3D ( 'NONE', #6540, #5312, #13228 ) ;
#7431 = CARTESIAN_POINT ( 'NONE',  ( 2.714587707229028535, -4.206234748388760991, -2.116820038483221662E-14 ) ) ;
#7432 = VECTOR ( 'NONE', #6836, 1000.000000000000000 ) ;
#7433 = EDGE_CURVE ( 'NONE', #721, #1722, #13215, .T. ) ;
#7434 = ORIENTED_EDGE ( 'NONE', *, *, #3430, .F. ) ;
#7435 = EDGE_LOOP ( 'NONE', ( #3302, #14235, #5409 ) ) ;
#7436 = DIRECTION ( 'NONE',  ( 0.000000000000000000, 0.000000000000000000, 1.000000000000000000 ) ) ;
#7437 = VERTEX_POINT ( 'NONE', #3333 ) ;
#7438 = EDGE_LOOP ( 'NONE', ( #6302, #8058, #6394, #757, #11181, #3359, #11732, #1268, #4536, #9883 ) ) ;
#7439 = MECHANICAL_DESIGN_GEOMETRIC_PRESENTATION_REPRESENTATION (  '', ( #6742 ), #11409 ) ;
#7440 = CARTESIAN_POINT ( 'NONE',  ( 129.3408537872138595, 189.5765550933606107, -9.000000000000007105 ) ) ;
#7441 = EDGE_CURVE ( 'NONE', #11064, #4271, #9097, .T. ) ;
#7442 = CARTESIAN_POINT ( 'NONE',  ( 0.000000000000000000, -3.031088913245536087, 1.750000000000001554 ) ) ;
#7443 = CARTESIAN_POINT ( 'NONE',  ( 2.015657056808820791, 48.24519377879725113, 0.5351343119442704133 ) ) ;
#7444 = CARTESIAN_POINT ( 'NONE',  ( -5.594483210025202879E-14, -5.773502691896268857, -0.5999999999999894307 ) ) ;
#7445 = CYLINDRICAL_SURFACE ( 'NONE', #11720, 2.500000000000002220 ) ;
#7446 = SHAPE_DEFINITION_REPRESENTATION ( #415, #2934 ) ;
#7447 = CARTESIAN_POINT ( 'NONE',  ( 4.630153689607063860, 0.000000000000000000, 0.000000000000000000 ) ) ;
#7448 = LINE ( 'NONE', #11931, #6340 ) ;
#7449 = ORIENTED_EDGE ( 'NONE', *, *, #3800, .T. ) ;
#7450 = CARTESIAN_POINT ( 'NONE',  ( 129.3408537872138595, 199.5765550933606107, -9.000000000000007105 ) ) ;
#7451 = EDGE_CURVE ( 'NONE', #3061, #3492, #7173, .T. ) ;
#7452 = ORIENTED_EDGE ( 'NONE', *, *, #13807, .F. ) ;
#7453 = EDGE_LOOP ( 'NONE', ( #11721, #2031 ) ) ;
#7454 = DIRECTION ( 'NONE',  ( -1.000000000000000000, 0.000000000000000000, 0.000000000000000000 ) ) ;
#7455 = DIRECTION ( 'NONE',  ( 0.000000000000000000, 0.000000000000000000, -1.000000000000000000 ) ) ;
#7456 = PRESENTATION_STYLE_ASSIGNMENT (( #10903 ) ) ;
#7457 = DIRECTION ( 'NONE',  ( 1.000000000000000000, 0.000000000000000000, 0.000000000000000000 ) ) ;
#7458 = CARTESIAN_POINT ( 'NONE',  ( 22.00000000000000355, 40.00000000000000711, 25.00000000000000000 ) ) ;
#7459 = EDGE_CURVE ( 'NONE', #4944, #13268, #7414, .T. ) ;
#7460 = CARTESIAN_POINT ( 'NONE',  ( 34.92765351673772045, 110.5971499970933536, -25.00000000000000000 ) ) ;
#7461 = VECTOR ( 'NONE', #7805, 1000.000000000000000 ) ;
#7462 = ORIENTED_EDGE ( 'NONE', *, *, #3613, .F. ) ;
#7463 = UNCERTAINTY_MEASURE_WITH_UNIT (LENGTH_MEASURE( 1.000000000000000082E-05 ), #12019, 'distance_accuracy_value', 'NONE');
#7464 = FACE_OUTER_BOUND ( 'NONE', #8096, .T. ) ;
#7465 = CARTESIAN_POINT ( 'NONE',  ( 92.68170757442806007, 124.5765550933605965, -25.00000000000000000 ) ) ;
#7466 = CARTESIAN_POINT ( 'NONE',  ( 1.560000000000005826, 0.000000000000000000, 0.000000000000000000 ) ) ;
#7467 = VERTEX_POINT ( 'NONE', #11078 ) ;
#7468 = CARTESIAN_POINT ( 'NONE',  ( -5.253368672218639013, -3.033033817057793957, -4.659491423763650886 ) ) ;
#7469 = DIRECTION ( 'NONE',  ( -1.000000000000000000, 0.000000000000000000, 0.000000000000000000 ) ) ;
#7470 = DIRECTION ( 'NONE',  ( 1.000000000000000000, 0.000000000000000000, 0.000000000000000000 ) ) ;
#7471 = ORIENTED_EDGE ( 'NONE', *, *, #6778, .F. ) ;
#7472 = AXIS2_PLACEMENT_3D ( 'NONE', #7421, #8380, #1657 ) ;
#7473 = DIRECTION ( 'NONE',  ( 0.000000000000000000, 1.000000000000000000, 0.000000000000000000 ) ) ;
#7474 = AXIS2_PLACEMENT_3D ( 'NONE', #2534, #2604, #8374 ) ;
#7475 = CARTESIAN_POINT ( 'NONE',  ( 0.5469803261926681204, -4.303002914946961077, -3.235259548911087357 ) ) ;
#7476 = ORIENTED_EDGE ( 'NONE', *, *, #5027, .F. ) ;
#7477 = FACE_OUTER_BOUND ( 'NONE', #10656, .T. ) ;
#7478 = EDGE_CURVE ( 'NONE', #1985, #3428, #6946, .T. ) ;
#7479 = DIRECTION ( 'NONE',  ( -1.000000000000000000, 0.000000000000000000, 0.000000000000000000 ) ) ;
#7480 = EDGE_CURVE ( 'NONE', #1777, #8457, #5118, .T. ) ;
#7481 = VERTEX_POINT ( 'NONE', #12254 ) ;
#7482 = CIRCLE ( 'NONE', #8890, 2.500000000000002220 ) ;
#7483 = COLOUR_RGB ( '', 0.08235294, 0.09019608, 0.10196078) ;
#7484 = ORIENTED_EDGE ( 'NONE', *, *, #12835, .F. ) ;
#7485 = CARTESIAN_POINT ( 'NONE',  ( 4.630153689607063860, 9.559099815976924059E-16, 5.371010071662830399 ) ) ;
#7486 = CARTESIAN_POINT ( 'NONE',  ( -4.000255272253210315, 47.42805584886342274, 3.737655343436113942 ) ) ;
#7487 = EDGE_LOOP ( 'NONE', ( #6290, #11515, #3096, #3528 ) ) ;
#7488 = VECTOR ( 'NONE', #9559, 1000.000000000000000 ) ;
#7489 = CARTESIAN_POINT ( 'NONE',  ( 4.175572532730952524, -4.122058607836128097, 1.176423331927875400E-14 ) ) ;
#7490 = DIRECTION ( 'NONE',  ( 0.000000000000000000, 0.000000000000000000, 1.000000000000000000 ) ) ;
#7491 = CARTESIAN_POINT ( 'NONE',  ( 61.53192852109764743, -5.819950020346492892, 25.00000000000000000 ) ) ;
#7492 = DIRECTION ( 'NONE',  ( -1.000000000000000000, 0.000000000000000000, 0.000000000000000000 ) ) ;
#7493 = EDGE_LOOP ( 'NONE', ( #1650, #9785, #3756, #1662, #11873, #9328, #2353 ) ) ;
#7494 = CARTESIAN_POINT ( 'NONE',  ( 88.22284556172391490, 29.57655509336062849, -117.0000000000000000 ) ) ;
#7495 = CARTESIAN_POINT ( 'NONE',  ( 4.630153689607063860, 0.000000000000000000, 0.000000000000000000 ) ) ;
#7496 = AXIS2_PLACEMENT_3D ( 'NONE', #2942, #6279, #9437 ) ;
#7497 = AXIS2_PLACEMENT_3D ( 'NONE', #10238, #4492, #2419 ) ;
#7498 = FACE_OUTER_BOUND ( 'NONE', #12663, .T. ) ;
#7499 = EDGE_LOOP ( 'NONE', ( #1434, #13339, #9382, #1256 ) ) ;
#7500 = EDGE_LOOP ( 'NONE', ( #833, #3712, #1195, #8893 ) ) ;
#7501 = B_SPLINE_CURVE_WITH_KNOTS ( 'NONE', 3,
 ( #13366, #5515, #10186, #111 ),
 .UNSPECIFIED., .F., .F.,
 ( 4, 4 ),
 ( 2.380737581874191823E-07, 0.002336974151641544283 ),
 .UNSPECIFIED. ) ;
#7502 = VERTEX_POINT ( 'NONE', #3186 ) ;
#7503 = CARTESIAN_POINT ( 'NONE',  ( 0.000000000000000000, 0.000000000000000000, -3.500000000000010214 ) ) ;
#7504 = ORIENTED_EDGE ( 'NONE', *, *, #10118, .F. ) ;
#7505 = VECTOR ( 'NONE', #5089, 1000.000000000000000 ) ;
#7506 = ORIENTED_EDGE ( 'NONE', *, *, #917, .T. ) ;
#7507 = LINE ( 'NONE', #5323, #11678 ) ;
#7508 = VECTOR ( 'NONE', #5135, 999.9999999999998863 ) ;
#7509 = VECTOR ( 'NONE', #9752, 1000.000000000000000 ) ;
#7510 = DIRECTION ( 'NONE',  ( 0.000000000000000000, 0.000000000000000000, -1.000000000000000000 ) ) ;
#7511 = DIRECTION ( 'NONE',  ( 0.000000000000000000, 0.000000000000000000, 1.000000000000000000 ) ) ;
#7512 = CARTESIAN_POINT ( 'NONE',  ( 76.68170757442801744, 39.57655509336063204, 33.00000000000000000 ) ) ;
#7513 = FACE_OUTER_BOUND ( 'NONE', #1216, .T. ) ;
#7514 = APPLICATION_PROTOCOL_DEFINITION ( 'draft international standard', 'automotive_design', 1998, #4309 ) ;
#7515 = CARTESIAN_POINT ( 'NONE',  ( 3.999999999999998224, 2.472263363263131009, -3.387027814857410224 ) ) ;
#7516 = B_SPLINE_CURVE_WITH_KNOTS ( 'NONE', 3,
 ( #1287, #2463, #6978, #6771, #3643, #8971 ),
 .UNSPECIFIED., .F., .F.,
 ( 4, 2, 4 ),
 ( 0.01471339550817208665, 0.01588188803962661128, 0.01705038057108113764 ),
 .UNSPECIFIED. ) ;
#7517 = EDGE_CURVE ( 'NONE', #5297, #13868, #5294, .T. ) ;
#7518 = FACE_OUTER_BOUND ( 'NONE', #6362, .T. ) ;
#7519 = PRESENTATION_LAYER_ASSIGNMENT (  '', '', ( #10328 ) ) ;
#7520 = VECTOR ( 'NONE', #1180, 1000.000000000000000 ) ;
#7521 = CARTESIAN_POINT ( 'NONE',  ( 37.35300976710104948, 100.8957249956400375, 25.00000000000000000 ) ) ;
#7522 = EDGE_CURVE ( 'NONE', #4685, #2107, #3012, .T. ) ;
#7523 = VERTEX_POINT ( 'NONE', #9756 ) ;
#7524 = EDGE_CURVE ( 'NONE', #4218, #13865, #26, .T. ) ;
#7525 = ORIENTED_EDGE ( 'NONE', *, *, #9870, .T. ) ;
#7526 = PLANE ( 'NONE',  #8039 ) ;
#7527 = ORIENTED_EDGE ( 'NONE', *, *, #5957, .F. ) ;
#7528 = DIRECTION ( 'NONE',  ( -1.000000000000000000, 0.000000000000000000, 0.000000000000000000 ) ) ;
#7529 = DIRECTION ( 'NONE',  ( 0.000000000000000000, 0.000000000000000000, -1.000000000000000000 ) ) ;
#7530 = STYLED_ITEM ( 'NONE', ( #548 ), #5243 ) ;
#7531 = DIRECTION ( 'NONE',  ( 1.000000000000000000, 0.000000000000000000, 0.000000000000000000 ) ) ;
#7532 = AXIS2_PLACEMENT_3D ( 'NONE', #7589, #3612, #4476 ) ;
#7533 = AXIS2_PLACEMENT_3D ( 'NONE', #9594, #9737, #13046 ) ;
#7534 = EDGE_CURVE ( 'NONE', #408, #2504, #5439, .T. ) ;
#7535 = ORIENTED_EDGE ( 'NONE', *, *, #5206, .F. ) ;
#7536 = VERTEX_POINT ( 'NONE', #14307 ) ;
#7537 = DIRECTION ( 'NONE',  ( 0.000000000000000000, 0.000000000000000000, 1.000000000000000000 ) ) ;
#7538 = CARTESIAN_POINT ( 'NONE',  ( -5.284804376168110274, -3.015249596956827816, -4.666192694417973463 ) ) ;
#7539 =( REPRESENTATION_RELATIONSHIP ('NONE','NONE', #10295, #5343 ) REPRESENTATION_RELATIONSHIP_WITH_TRANSFORMATION ( #7585 )SHAPE_REPRESENTATION_RELATIONSHIP( ) );
#7540 = VECTOR ( 'NONE', #3689, 1000.000000000000000 ) ;
#7541 = DIRECTION ( 'NONE',  ( -0.2425356250363328581, 0.9701425001453318764, 0.000000000000000000 ) ) ;
#7542 = AXIS2_PLACEMENT_3D ( 'NONE', #11395, #9122, #12365 ) ;
#7543 = CARTESIAN_POINT ( 'NONE',  ( 22.00000000000000000, 67.00000000000000000, 25.00000000000000000 ) ) ;
#7544 = LINE ( 'NONE', #11810, #2958 ) ;
#7545 = DIRECTION ( 'NONE',  ( 1.000000000000000000, 0.000000000000000000, 0.000000000000000000 ) ) ;
#7546 = LINE ( 'NONE', #8653, #11702 ) ;
#7547 = LINE ( 'NONE', #12034, #5139 ) ;
#7548 = PLANE ( 'NONE',  #14031 ) ;
#7549 = ADVANCED_FACE ( 'NONE', ( #8801 ), #8732, .T. ) ;
#7550 = DIRECTION ( 'NONE',  ( 0.000000000000000000, -1.000000000000000000, 0.000000000000000000 ) ) ;
#7551 = ORIENTED_EDGE ( 'NONE', *, *, #1343, .F. ) ;
#7552 = VERTEX_POINT ( 'NONE', #1121 ) ;
#7553 = CARTESIAN_POINT ( 'NONE',  ( 64.03192852109765454, -5.819950020346492892, -25.00000000000000000 ) ) ;
#7554 = CYLINDRICAL_SURFACE ( 'NONE', #4045, 2.500000000000000444 ) ;
#7555 = VECTOR ( 'NONE', #8056, 1000.000000000000000 ) ;
#7556 = ORIENTED_EDGE ( 'NONE', *, *, #1838, .T. ) ;
#7557 = CARTESIAN_POINT ( 'NONE',  ( -140.0000000000003411, 189.5765550933606107, 47.99999999999998579 ) ) ;
#7558 = CARTESIAN_POINT ( 'NONE',  ( 88.22284556172391490, -83.66032599071898801, -28.00000000000000000 ) ) ;
#7559 = VERTEX_POINT ( 'NONE', #10046 ) ;
#7560 = ORIENTED_EDGE ( 'NONE', *, *, #8716, .F. ) ;
#7561 = LINE ( 'NONE', #14318, #10846 ) ;
#7562 = LINE ( 'NONE', #6330, #7505 ) ;
#7563 = EDGE_LOOP ( 'NONE', ( #4338, #12537, #11369, #2984 ) ) ;
#7564 = CARTESIAN_POINT ( 'NONE',  ( 4.158921614371306141, 1.986121848748767071, -3.559936047944508797 ) ) ;
#7565 = DIRECTION ( 'NONE',  ( 0.000000000000000000, 0.000000000000000000, -1.000000000000000000 ) ) ;
#7566 = CARTESIAN_POINT ( 'NONE',  ( 59.10586122665984732, -20.42344490663941414, 35.00000000000000000 ) ) ;
#7567 = ADVANCED_FACE ( 'NONE', ( #8942 ), #14445, .T. ) ;
#7568 = CARTESIAN_POINT ( 'NONE',  ( 64.10657227073433262, 3.881474981106830757, 25.00000000000000000 ) ) ;
#7569 = ORIENTED_EDGE ( 'NONE', *, *, #37, .T. ) ;
#7570 = PRODUCT_RELATED_PRODUCT_CATEGORY ( 'part', '', ( #8232 ) ) ;
#7571 = EDGE_CURVE ( 'NONE', #3393, #3463, #2078, .T. ) ;
#7572 =( LENGTH_UNIT ( ) NAMED_UNIT ( * ) SI_UNIT ( .MILLI., .METRE. ) );
#7573 = FACE_OUTER_BOUND ( 'NONE', #8865, .T. ) ;
#7574 = FACE_OUTER_BOUND ( 'NONE', #7896, .T. ) ;
#7575 = AXIS2_PLACEMENT_3D ( 'NONE', #6498, #3226, #10835 ) ;
#7576 = ORIENTED_EDGE ( 'NONE', *, *, #7161, .F. ) ;
#7577 = ORIENTED_EDGE ( 'NONE', *, *, #8108, .F. ) ;
#7578 = DIRECTION ( 'NONE',  ( -0.000000000000000000, -0.000000000000000000, -1.000000000000000000 ) ) ;
#7579 = ORIENTED_EDGE ( 'NONE', *, *, #8753, .F. ) ;
#7580 = CARTESIAN_POINT ( 'NONE',  ( -18.12748877629581656, 43.82334295289051340, 0.000000000000000000 ) ) ;
#7581 = FACE_BOUND ( 'NONE', #6203, .T. ) ;
#7582 = CARTESIAN_POINT ( 'NONE',  ( 4.000255272253209426, 47.42805584886342274, 3.737655343436113498 ) ) ;
#7583 = CARTESIAN_POINT ( 'NONE',  ( 0.000000000000000000, -4.618802153517030717, -4.699999999999981526 ) ) ;
#7584 = CARTESIAN_POINT ( 'NONE',  ( 5.684607805603219362E-18, 1.387778780781445182E-16, 2.499999999999999112 ) ) ;
#7585 = ITEM_DEFINED_TRANSFORMATION ( 'NONE', 'NONE', #11300,  #11025 ) ;
#7586 = DIRECTION ( 'NONE',  ( 0.000000000000000000, 0.000000000000000000, 1.000000000000000000 ) ) ;
#7587 = CARTESIAN_POINT ( 'NONE',  ( 4.086262629614033415, -4.082406995609999534, -0.07093633357112584525 ) ) ;
#7588 = EDGE_LOOP ( 'NONE', ( #9699, #12550, #14101, #3020 ) ) ;
#7589 = CARTESIAN_POINT ( 'NONE',  ( 108.6817075744280316, 69.57655509336046862, 0.000000000000000000 ) ) ;
#7590 = ORIENTED_EDGE ( 'NONE', *, *, #7969, .T. ) ;
#7591 = ORIENTED_EDGE ( 'NONE', *, *, #10402, .F. ) ;
#7592 = ORIENTED_EDGE ( 'NONE', *, *, #9187, .F. ) ;
#7593 = AXIS2_PLACEMENT_3D ( 'NONE', #745, #1773, #6063 ) ;
#7594 = CARTESIAN_POINT ( 'NONE',  ( 2.369999999999996998, 0.000000000000000000, 0.000000000000000000 ) ) ;
#7595 = CARTESIAN_POINT ( 'NONE',  ( 5.000000000000000888, 2.424500739214346723, -0.4207179063848164313 ) ) ;
#7596 = LINE ( 'NONE', #1167, #3531 ) ;
#7597 = CYLINDRICAL_SURFACE ( 'NONE', #10192, 4.000000000000000000 ) ;
#7598 = FILL_AREA_STYLE_COLOUR ( '', #4020 ) ;
#7599 = ADVANCED_FACE ( 'NONE', ( #13148 ), #12037, .T. ) ;
#7600 = VERTEX_POINT ( 'NONE', #896 ) ;
#7601 = CARTESIAN_POINT ( 'NONE',  ( -4.106788408769115985E-15, -2.686816014504578298, -2.346298152288348149 ) ) ;
#7602 = DIRECTION ( 'NONE',  ( 0.000000000000000000, 0.000000000000000000, -1.000000000000000000 ) ) ;
#7603 = ADVANCED_FACE ( 'NONE', ( #5366 ), #10994, .T. ) ;
#7604 = DIRECTION ( 'NONE',  ( -1.000000000000000000, -1.665334536937734071E-16, 0.000000000000000000 ) ) ;
#7605 = LINE ( 'NONE', #10246, #6086 ) ;
#7606 = ADVANCED_FACE ( 'NONE', ( #9010 ), #11422, .T. ) ;
#7607 = PRODUCT_DEFINITION_CONTEXT ( 'detailed design', #4309, 'design' ) ;
#7608 = LINE ( 'NONE', #887, #7953 ) ;
#7609 = CARTESIAN_POINT ( 'NONE',  ( 20.00000000000000000, 37.00000000000000711, -25.00000000000000000 ) ) ;
#7610 = DIRECTION ( 'NONE',  ( 0.000000000000000000, -1.000000000000000000, 0.000000000000000000 ) ) ;
#7611 = CARTESIAN_POINT ( 'NONE',  ( 0.000000000000000000, 0.000000000000000000, -25.00000000000000000 ) ) ;
#7612 = DIRECTION ( 'NONE',  ( 1.000000000000000000, 0.000000000000000000, 0.000000000000000000 ) ) ;
#7613 = ADVANCED_FACE ( 'NONE', ( #1480 ), #13570, .T. ) ;
#7614 = DIRECTION ( 'NONE',  ( -4.625929269271486900E-16, 1.000000000000000000, 0.000000000000000000 ) ) ;
#7615 = ORIENTED_EDGE ( 'NONE', *, *, #7818, .F. ) ;
#7616 = CARTESIAN_POINT ( 'NONE',  ( 5.000000000000002665, 1.924500897298742963, -4.118275046351175916 ) ) ;
#7617 = VERTEX_POINT ( 'NONE', #10250 ) ;
#7618 = LINE ( 'NONE', #9832, #166 ) ;
#7619 = FACE_BOUND ( 'NONE', #1055, .T. ) ;
#7620 = ORIENTED_EDGE ( 'NONE', *, *, #6681, .T. ) ;
#7621 = EDGE_LOOP ( 'NONE', ( #8489, #5630, #545, #2535 ) ) ;
#7622 = ADVANCED_FACE ( 'NONE', ( #3546 ), #9154, .F. ) ;
#7623 = ORIENTED_EDGE ( 'NONE', *, *, #13681, .F. ) ;
#7624 = AXIS2_PLACEMENT_3D ( 'NONE', #1169, #3169, #14429 ) ;
#7625 = DIRECTION ( 'NONE',  ( 1.000000000000000000, 0.000000000000000000, 0.000000000000000000 ) ) ;
#7626 = CARTESIAN_POINT ( 'NONE',  ( 108.6817075744280174, -30.42344490663958112, 47.99999999999998579 ) ) ;
#7627 = AXIS2_PLACEMENT_3D ( 'NONE', #13732, #2755, #13671 ) ;
#7628 = CARTESIAN_POINT ( 'NONE',  ( 4.086262629614031638, -1.979770830881089738, -3.570936333571117505 ) ) ;
#7629 = CARTESIAN_POINT ( 'NONE',  ( 58.68170757442803165, 34.50422595846454499, 28.00000000000000000 ) ) ;
#7630 = VECTOR ( 'NONE', #10588, 1000.000000000000000 ) ;
#7631 = DIRECTION ( 'NONE',  ( 0.000000000000000000, 0.000000000000000000, 1.000000000000000000 ) ) ;
#7632 = LINE ( 'NONE', #6617, #11174 ) ;
#7633 = EDGE_CURVE ( 'NONE', #10272, #5482, #314, .T. ) ;
#7634 = ORIENTED_EDGE ( 'NONE', *, *, #8828, .T. ) ;
#7635 =( NAMED_UNIT ( * ) SI_UNIT ( $, .STERADIAN. ) SOLID_ANGLE_UNIT ( ) );
#7636 = CARTESIAN_POINT ( 'NONE',  ( 59.10586122665984732, -20.42344490663941414, 35.00000000000000000 ) ) ;
#7637 = CARTESIAN_POINT ( 'NONE',  ( 4.030867648405330073, 3.732851566702002799, 0.5345114293581457732 ) ) ;
#7638 = AXIS2_PLACEMENT_3D ( 'NONE', #9697, #14169, #972 ) ;
#7639 = VECTOR ( 'NONE', #12628, 1000.000000000000000 ) ;
#7640 = ORIENTED_EDGE ( 'NONE', *, *, #11197, .T. ) ;
#7641 = ORIENTED_EDGE ( 'NONE', *, *, #6220, .T. ) ;
#7642 = EDGE_CURVE ( 'NONE', #7974, #10568, #11212, .T. ) ;
#7643 = CARTESIAN_POINT ( 'NONE',  ( 56.99999999999997868, -1.031959805901694782E-15, -23.00000000000000000 ) ) ;
#7644 = EDGE_LOOP ( 'NONE', ( #8775, #245, #8419, #14364 ) ) ;
#7645 = CARTESIAN_POINT ( 'NONE',  ( 18.12748877629582367, 43.82334295289049919, 0.000000000000000000 ) ) ;
#7646 = DIRECTION ( 'NONE',  ( 0.000000000000000000, 0.000000000000000000, 1.000000000000000000 ) ) ;
#7647 = AXIS2_PLACEMENT_3D ( 'NONE', #11945, #13201, #2218 ) ;
#7648 = CARTESIAN_POINT ( 'NONE',  ( 22.00000000000000000, 80.00000000000000000, 25.00000000000000000 ) ) ;
#7649 = CIRCLE ( 'NONE', #7888, 3.499999999999999112 ) ;
#7650 = CARTESIAN_POINT ( 'NONE',  ( 20.00000000000000355, 40.00000000000000711, -25.00000000000000000 ) ) ;
#7651 = CIRCLE ( 'NONE', #9777, 13.00000000000002487 ) ;
#7652 = CARTESIAN_POINT ( 'NONE',  ( 2.100000000000000089, 3.497202527569242018E-16, -4.394516984716101859 ) ) ;
#7653 = CARTESIAN_POINT ( 'NONE',  ( 56.99999999999997868, -1.031959805901694782E-15, 23.00000000000000000 ) ) ;
#7654 = CARTESIAN_POINT ( 'NONE',  ( 5.091953023115924459, -4.682427078960499145, -1.387922423807041543E-14 ) ) ;
#7655 = VERTEX_POINT ( 'NONE', #12390 ) ;
#7656 = DIRECTION ( 'NONE',  ( 0.000000000000000000, 0.000000000000000000, -1.000000000000000000 ) ) ;
#7657 = ORIENTED_EDGE ( 'NONE', *, *, #1851, .F. ) ;
#7658 = VERTEX_POINT ( 'NONE', #4639 ) ;
#7659 = EDGE_CURVE ( 'NONE', #9307, #10589, #11218, .T. ) ;
#7660 = MECHANICAL_DESIGN_GEOMETRIC_PRESENTATION_REPRESENTATION (  '', ( #14006 ), #4202 ) ;
#7661 = ADVANCED_FACE ( 'NONE', ( #2499 ), #10930, .T. ) ;
#7662 = LINE ( 'NONE', #12224, #9924 ) ;
#7663 = B_SPLINE_CURVE_WITH_KNOTS ( 'NONE', 3,
 ( #9969, #8790, #4355, #13272, #3248 ),
 .UNSPECIFIED., .F., .F.,
 ( 4, 1, 4 ),
 ( 0.000000000000000000, 0.002309401076758503622, 0.004618802153517006376 ),
 .UNSPECIFIED. ) ;
#7664 = ORIENTED_EDGE ( 'NONE', *, *, #9005, .T. ) ;
#7665 = SURFACE_STYLE_USAGE ( .BOTH. , #12367 ) ;
#7666 = DIRECTION ( 'NONE',  ( 1.000000000000000000, -2.551526159633733968E-19, -1.987661601597216239E-18 ) ) ;
#7667 = CARTESIAN_POINT ( 'NONE',  ( 0.000000000000000000, 25.49999999999996803, 8.000000000000007105 ) ) ;
#7668 = ADVANCED_FACE ( 'NONE', ( #7985 ), #12460, .T. ) ;
#7669 = ORIENTED_EDGE ( 'NONE', *, *, #14316, .T. ) ;
#7670 = CARTESIAN_POINT ( 'NONE',  ( 5.108576461337686503, 4.721997478884313537, 0.02371338167649103892 ) ) ;
#7671 = DIRECTION ( 'NONE',  ( 0.000000000000000000, 0.000000000000000000, 1.000000000000000000 ) ) ;
#7672 = SURFACE_STYLE_FILL_AREA ( #5346 ) ;
#7673 = CARTESIAN_POINT ( 'NONE',  ( 0.000000000000000000, 0.000000000000000000, -0.3501037691048258793 ) ) ;
#7674 = AXIS2_PLACEMENT_3D ( 'NONE', #7719, #3356, #12338 ) ;
#7675 = ORIENTED_EDGE ( 'NONE', *, *, #8384, .T. ) ;
#7676 = ORIENTED_EDGE ( 'NONE', *, *, #11540, .T. ) ;
#7677 = CARTESIAN_POINT ( 'NONE',  ( 0.3572655899081733644, 2.309401076758511806, 3.999999999999989786 ) ) ;
#7678 = DIRECTION ( 'NONE',  ( 0.000000000000000000, 0.000000000000000000, 1.000000000000000000 ) ) ;
#7679 = VECTOR ( 'NONE', #8621, 1000.000000000000000 ) ;
#7680 = CARTESIAN_POINT ( 'NONE',  ( 40.00000000000000711, 80.00000000000000000, 25.00000000000000000 ) ) ;
#7681 = EDGE_LOOP ( 'NONE', ( #11198, #13544, #8051, #13200, #11094 ) ) ;
#7682 = EDGE_CURVE ( 'NONE', #6682, #13714, #12808, .T. ) ;
#7683 = EDGE_CURVE ( 'NONE', #1123, #9662, #6886, .T. ) ;
#7684 = CARTESIAN_POINT ( 'NONE',  ( -1.274241539467172002, -3.883118457693044423, -2.920601398289143003 ) ) ;
#7685 = B_SPLINE_CURVE_WITH_KNOTS ( 'NONE', 3,
 ( #7468, #12920, #7402, #8514, #6167, #693 ),
 .UNSPECIFIED., .F., .F.,
 ( 4, 2, 4 ),
 ( 0.000000000000000000, 0.001529397995383623013, 0.003058795990767246026 ),
 .UNSPECIFIED. ) ;
#7686 = AXIS2_PLACEMENT_3D ( 'NONE', #12067, #5263, #13179 ) ;
#7687 = CARTESIAN_POINT ( 'NONE',  ( 27.57694101601105530, 130.0000000000000000, -25.00000000000000000 ) ) ;
#7688 = CARTESIAN_POINT ( 'NONE',  ( -129.3408537872145132, 199.5765550933606107, -75.00000000000001421 ) ) ;
#7689 = LINE ( 'NONE', #4504, #5060 ) ;
#7690 = CARTESIAN_POINT ( 'NONE',  ( 2.749999999999998224, 3.306546357697852747E-16, -2.699999999999999289 ) ) ;
#7691 = FACE_OUTER_BOUND ( 'NONE', #10255, .T. ) ;
#7692 = VECTOR ( 'NONE', #13194, 1000.000000000000000 ) ;
#7693 = SURFACE_SIDE_STYLE ('',( #5362 ) ) ;
#7694 = PLANE ( 'NONE',  #7292 ) ;
#7695 = EDGE_LOOP ( 'NONE', ( #5832, #2407, #14252, #11921 ) ) ;
#7696 = ORIENTED_EDGE ( 'NONE', *, *, #11713, .F. ) ;
#7697 = DIRECTION ( 'NONE',  ( 0.000000000000000000, 0.000000000000000000, -1.000000000000000000 ) ) ;
#7698 = EDGE_CURVE ( 'NONE', #6127, #2739, #106, .T. ) ;
#7699 = VECTOR ( 'NONE', #10306, 1000.000000000000000 ) ;
#7700 = ORIENTED_EDGE ( 'NONE', *, *, #5510, .F. ) ;
#7701 = DIRECTION ( 'NONE',  ( -0.000000000000000000, -1.000000000000000000, 0.000000000000000000 ) ) ;
#7702 = CARTESIAN_POINT ( 'NONE',  ( 0.000000000000000000, -3.031088913245536087, 1.750000000000001554 ) ) ;
#7703 = EDGE_CURVE ( 'NONE', #6826, #4679, #10005, .T. ) ;
#7704 = ADVANCED_FACE ( 'NONE', ( #10333, #7025, #13649 ), #6954, .F. ) ;
#7705 = VERTEX_POINT ( 'NONE', #12589 ) ;
#7706 = ORIENTED_EDGE ( 'NONE', *, *, #3890, .F. ) ;
#7707 = CARTESIAN_POINT ( 'NONE',  ( 4.071447262713911996, -2.020725942163681399, -3.500000000000010214 ) ) ;
#7708 = FACE_OUTER_BOUND ( 'NONE', #12814, .T. ) ;
#7709 = ADVANCED_FACE ( 'NONE', ( #12521 ), #1395, .T. ) ;
#7710 = CARTESIAN_POINT ( 'NONE',  ( 4.180345304246198879, -4.135116856707401922, 0.02129519942689507561 ) ) ;
#7711 = VECTOR ( 'NONE', #8020, 1000.000000000000000 ) ;
#7712 = LINE ( 'NONE', #2170, #12809 ) ;
#7713 = VECTOR ( 'NONE', #1635, 1000.000000000000114 ) ;
#7714 = CARTESIAN_POINT ( 'NONE',  ( -108.6817075744279890, 189.5765550933605823, -106.9999999999999858 ) ) ;
#7715 = EDGE_CURVE ( 'NONE', #10509, #12288, #13760, .T. ) ;
#7716 = CARTESIAN_POINT ( 'NONE',  ( 68.68170757442801744, 29.57655509336062849, 33.00000000000002842 ) ) ;
#7717 = ORIENTED_EDGE ( 'NONE', *, *, #4834, .F. ) ;
#7718 = FILL_AREA_STYLE_COLOUR ( '', #7483 ) ;
#7719 = CARTESIAN_POINT ( 'NONE',  ( 6.800000000000028244, -6.938893903907228378E-15, 0.000000000000000000 ) ) ;
#7720 = EDGE_CURVE ( 'NONE', #3991, #4685, #10552, .T. ) ;
#7721 = LINE ( 'NONE', #6693, #6242 ) ;
#7722 = AXIS2_PLACEMENT_3D ( 'NONE', #579, #2697, #8305 ) ;
#7723 = EDGE_LOOP ( 'NONE', ( #7221, #5950 ) ) ;
#7724 = AXIS2_PLACEMENT_3D ( 'NONE', #13205, #6380, #1785 ) ;
#7725 = ORIENTED_EDGE ( 'NONE', *, *, #13188, .F. ) ;
#7726 = CARTESIAN_POINT ( 'NONE',  ( 28.00000000000000355, 24.50000000000001421, 8.000000000000007105 ) ) ;
#7727 = VERTEX_POINT ( 'NONE', #12742 ) ;
#7728 = FACE_OUTER_BOUND ( 'NONE', #4335, .T. ) ;
#7729 = FACE_OUTER_BOUND ( 'NONE', #8267, .T. ) ;
#7730 = SURFACE_STYLE_USAGE ( .BOTH. , #10214 ) ;
#7731 = AXIS2_PLACEMENT_3D ( 'NONE', #11337, #9208, #3600 ) ;
#7732 = CARTESIAN_POINT ( 'NONE',  ( 108.6817075744280743, 124.5765550933606107, 25.00000000000000000 ) ) ;
#7733 = CARTESIAN_POINT ( 'NONE',  ( 59.10586122665984732, -20.42344490663941414, -35.00000000000000000 ) ) ;
#7734 = CARTESIAN_POINT ( 'NONE',  ( 108.6817075744280174, 69.57655509336049704, 1.592040838891559450E-14 ) ) ;
#7735 = EDGE_CURVE ( 'NONE', #10580, #6578, #3837, .T. ) ;
#7736 = CARTESIAN_POINT ( 'NONE',  ( 3.958484000408148518, -2.327740518749091159, 2.968235154689833344 ) ) ;
#7737 = ORIENTED_EDGE ( 'NONE', *, *, #7274, .T. ) ;
#7738 = B_SPLINE_CURVE_WITH_KNOTS ( 'NONE', 3,
 ( #4909, #11637, #5202, #1698, #11942, #6148 ),
 .UNSPECIFIED., .F., .F.,
 ( 4, 2, 4 ),
 ( -3.640115492426956241E-06, 0.0002066546034006362231, 0.0004169493222936994413 ),
 .UNSPECIFIED. ) ;
#7739 = CARTESIAN_POINT ( 'NONE',  ( 76.68170757442798902, 124.5765550933606249, 25.00000000000000000 ) ) ;
#7740 = VERTEX_POINT ( 'NONE', #684 ) ;
#7741 = ORIENTED_EDGE ( 'NONE', *, *, #14050, .F. ) ;
#7742 = VECTOR ( 'NONE', #13313, 1000.000000000000000 ) ;
#7743 = ORIENTED_EDGE ( 'NONE', *, *, #14366, .F. ) ;
#7744 = AXIS2_PLACEMENT_3D ( 'NONE', #2699, #11464, #8024 ) ;
#7745 = VECTOR ( 'NONE', #11176, 1000.000000000000000 ) ;
#7746 = CARTESIAN_POINT ( 'NONE',  ( 3.822382184081044798, 10.25936179483148969, 8.000000000000007105 ) ) ;
#7747 = VERTEX_POINT ( 'NONE', #8269 ) ;
#7748 = ORIENTED_EDGE ( 'NONE', *, *, #11297, .F. ) ;
#7749 = DIRECTION ( 'NONE',  ( 1.734723475976770502E-18, -4.440892098500621231E-16, -1.000000000000000000 ) ) ;
#7750 = CARTESIAN_POINT ( 'NONE',  ( -0.8653900595644484772, 5.556556492855584395, -4.490801088233111749 ) ) ;
#7751 = CARTESIAN_POINT ( 'NONE',  ( -129.3408537872145132, 199.5765550933606107, -4.000000000000031086 ) ) ;
#7752 = CARTESIAN_POINT ( 'NONE',  ( 5.000000000000000000, -2.886751345948148639, -4.284345921091780696 ) ) ;
#7753 = CYLINDRICAL_SURFACE ( 'NONE', #4506, 3.299999999999976730 ) ;
#7754 = DIRECTION ( 'NONE',  ( 1.000000000000000000, 0.000000000000000000, 0.000000000000000000 ) ) ;
#7755 = AXIS2_PLACEMENT_3D ( 'NONE', #9698, #7410, #703 ) ;
#7756 = ADVANCED_FACE ( 'NONE', ( #8341 ), #12987, .F. ) ;
#7757 = DIRECTION ( 'NONE',  ( 0.000000000000000000, 0.000000000000000000, 1.000000000000000000 ) ) ;
#7758 = VERTEX_POINT ( 'NONE', #12825 ) ;
#7759 = AXIS2_PLACEMENT_3D ( 'NONE', #2959, #3107, #9531 ) ;
#7760 = AXIS2_PLACEMENT_3D ( 'NONE', #10021, #5344, #8921 ) ;
#7761 = PRODUCT_DEFINITION ( 'UNKNOWN', '', #5236, #885 ) ;
#7762 = EDGE_CURVE ( 'NONE', #7552, #6880, #2808, .T. ) ;
#7763 = ORIENTED_EDGE ( 'NONE', *, *, #8065, .T. ) ;
#7764 = CARTESIAN_POINT ( 'NONE',  ( 0.3126073911695614882, -2.020725942163792421, -3.500000000000003109 ) ) ;
#7765 = CARTESIAN_POINT ( 'NONE',  ( 0.000000000000000000, 0.000000000000000000, 0.000000000000000000 ) ) ;
#7766 = CARTESIAN_POINT ( 'NONE',  ( 6.800000000000028244, -6.938893903907228378E-15, 0.000000000000000000 ) ) ;
#7767 = ORIENTED_EDGE ( 'NONE', *, *, #9715, .T. ) ;
#7768 = CARTESIAN_POINT ( 'NONE',  ( -2.836862643238879489, -3.208966885971408445, -3.205052026701902257 ) ) ;
#7769 = VECTOR ( 'NONE', #12159, 1000.000000000000000 ) ;
#7770 = AXIS2_PLACEMENT_3D ( 'NONE', #13694, #8033, #10385 ) ;
#7771 = CARTESIAN_POINT ( 'NONE',  ( 4.873329151231311052, -3.940175375302611638, 1.320232820537113216 ) ) ;
#7772 = DIRECTION ( 'NONE',  ( -1.000000000000000000, 0.000000000000000000, 0.000000000000000000 ) ) ;
#7773 = CARTESIAN_POINT ( 'NONE',  ( -2.100000000000000089, -9.254442493598001840E-17, -4.394516984716101859 ) ) ;
#7774 = CARTESIAN_POINT ( 'NONE',  ( 4.050823680195248855, -2.400527758044911142, -2.978030508226159778 ) ) ;
#7775 = ORIENTED_EDGE ( 'NONE', *, *, #10209, .T. ) ;
#7776 = ORIENTED_EDGE ( 'NONE', *, *, #7793, .T. ) ;
#7777 = DIRECTION ( 'NONE',  ( -1.000000000000000000, 2.551526159633733968E-19, 1.987661601597216239E-18 ) ) ;
#7778 = AXIS2_PLACEMENT_3D ( 'NONE', #13575, #7987, #12464 ) ;
#7779 = ORIENTED_EDGE ( 'NONE', *, *, #5427, .T. ) ;
#7780 = CARTESIAN_POINT ( 'NONE',  ( -0.8333333333333305948, 5.292377467571583338, -4.118275046351175028 ) ) ;
#7781 = PLANE ( 'NONE',  #7778 ) ;
#7782 = ORIENTED_EDGE ( 'NONE', *, *, #2723, .F. ) ;
#7783 = LINE ( 'NONE', #11219, #14361 ) ;
#7784 = CARTESIAN_POINT ( 'NONE',  ( 60.00000000000000000, -6.123233995736768255E-16, -25.00000000000000000 ) ) ;
#7785 = DIRECTION ( 'NONE',  ( -0.000000000000000000, 1.000000000000000000, 0.000000000000000000 ) ) ;
#7786 = DIRECTION ( 'NONE',  ( 0.000000000000000000, 0.000000000000000000, -1.000000000000000000 ) ) ;
#7787 = CARTESIAN_POINT ( 'NONE',  ( 5.599999999999994316, -4.041451884327377009, 0.000000000000000000 ) ) ;
#7788 = CARTESIAN_POINT ( 'NONE',  ( 4.050536630291712292, 2.401306687817035268, -2.976670123173770222 ) ) ;
#7789 = ORIENTED_EDGE ( 'NONE', *, *, #3599, .T. ) ;
#7790 =( NAMED_UNIT ( * ) SI_UNIT ( $, .STERADIAN. ) SOLID_ANGLE_UNIT ( ) );
#7791 = CIRCLE ( 'NONE', #3378, 2.500000000000002220 ) ;
#7792 = EDGE_CURVE ( 'NONE', #13250, #3003, #1704, .T. ) ;
#7793 = EDGE_CURVE ( 'NONE', #6124, #12192, #12904, .T. ) ;
#7794 = EDGE_LOOP ( 'NONE', ( #895, #6256, #8576, #11738 ) ) ;
#7795 = DIRECTION ( 'NONE',  ( 1.000000000000000000, 0.000000000000000000, 0.000000000000000000 ) ) ;
#7796 = DIRECTION ( 'NONE',  ( 1.000000000000000000, 0.000000000000000000, 0.000000000000000000 ) ) ;
#7797 = AXIS2_PLACEMENT_3D ( 'NONE', #1684, #13985, #4824 ) ;
#7798 = ORIENTED_EDGE ( 'NONE', *, *, #2702, .F. ) ;
#7799 = ORIENTED_EDGE ( 'NONE', *, *, #1844, .F. ) ;
#7800 = EDGE_LOOP ( 'NONE', ( #4245, #3102, #362, #11340 ) ) ;
#7801 = VECTOR ( 'NONE', #4537, 1000.000000000000000 ) ;
#7802 = DIRECTION ( 'NONE',  ( -1.000000000000000000, 0.000000000000000000, 0.000000000000000000 ) ) ;
#7803 = EDGE_CURVE ( 'NONE', #3245, #1176, #5134, .T. ) ;
#7804 = ORIENTED_EDGE ( 'NONE', *, *, #11283, .T. ) ;
#7805 = DIRECTION ( 'NONE',  ( -0.9240638205168503205, 0.3822382184081049017, 0.000000000000000000 ) ) ;
#7806 = DIRECTION ( 'NONE',  ( 0.000000000000000000, 8.482162385747133845E-47, -1.000000000000000000 ) ) ;
#7807 = EDGE_LOOP ( 'NONE', ( #12734, #105, #13490, #10440 ) ) ;
#7808 = CARTESIAN_POINT ( 'NONE',  ( 1.734723475976807094E-14, 35.49999999999996447, 0.000000000000000000 ) ) ;
#7809 = DIRECTION ( 'NONE',  ( 0.000000000000000000, 0.000000000000000000, -1.000000000000000000 ) ) ;
#7810 = CARTESIAN_POINT ( 'NONE',  ( 3.973514160553479613, 2.741076955031366058, 2.383932505289871884 ) ) ;
#7811 = EDGE_CURVE ( 'NONE', #4126, #1525, #752, .T. ) ;
#7812 = CARTESIAN_POINT ( 'NONE',  ( -5.253368672218636348, 3.033033817057773085, -4.659491423763650886 ) ) ;
#7813 = CARTESIAN_POINT ( 'NONE',  ( 4.030867648405613402, -2.329326259788630171, 2.965488570640940846 ) ) ;
#7814 = CLOSED_SHELL ( 'NONE', ( #6199, #8249, #3750, #3476, #12271, #10814 ) ) ;
#7815 = LINE ( 'NONE', #2046, #5440 ) ;
#7816 = ORIENTED_EDGE ( 'NONE', *, *, #6596, .F. ) ;
#7817 = ORIENTED_EDGE ( 'NONE', *, *, #7517, .F. ) ;
#7818 = EDGE_CURVE ( 'NONE', #7871, #5249, #11725, .T. ) ;
#7819 = ORIENTED_EDGE ( 'NONE', *, *, #799, .T. ) ;
#7820 = LINE ( 'NONE', #3383, #13078 ) ;
#7821 = CARTESIAN_POINT ( 'NONE',  ( -2.749999999999997780, 25.49999999999996803, 0.000000000000000000 ) ) ;
#7822 = CARTESIAN_POINT ( 'NONE',  ( 5.000000000000001776, 1.231908430319626602, -0.1119772403577116160 ) ) ;
#7823 = APPLICATION_CONTEXT ( 'automotive_design' ) ;
#7824 = FACE_OUTER_BOUND ( 'NONE', #4999, .T. ) ;
#7825 = CARTESIAN_POINT ( 'NONE',  ( 0.000000000000000000, 0.000000000000000000, 0.000000000000000000 ) ) ;
#7826 = CARTESIAN_POINT ( 'NONE',  ( 62.10586122665984732, -20.42344490663941414, -23.00000000000000000 ) ) ;
#7827 = CARTESIAN_POINT ( 'NONE',  ( 0.000000000000000000, 0.000000000000000000, 0.000000000000000000 ) ) ;
#7828 = DIRECTION ( 'NONE',  ( 0.000000000000000000, 0.000000000000000000, 1.000000000000000000 ) ) ;
#7829 = ORIENTED_EDGE ( 'NONE', *, *, #3947, .F. ) ;
#7830 = ORIENTED_EDGE ( 'NONE', *, *, #1624, .T. ) ;
#7831 = DIRECTION ( 'NONE',  ( 0.000000000000000000, -1.000000000000000000, 0.000000000000000000 ) ) ;
#7832 = CARTESIAN_POINT ( 'NONE',  ( 20.00000000000000355, 40.00000000000000711, -25.00000000000000000 ) ) ;
#7833 = DIRECTION ( 'NONE',  ( -1.000000000000000000, 2.551526159633733968E-19, 1.987661601597216239E-18 ) ) ;
#7834 = CARTESIAN_POINT ( 'NONE',  ( -2.742797192660130001, -3.035247456002393651, -3.133250573521596749 ) ) ;
#7835 = EDGE_CURVE ( 'NONE', #13588, #2847, #1620, .T. ) ;
#7836 = ADVANCED_FACE ( 'NONE', ( #6155 ), #2732, .T. ) ;
#7837 = CARTESIAN_POINT ( 'NONE',  ( 129.3408537872138595, 189.5765550933606107, -9.000000000000007105 ) ) ;
#7838 = CARTESIAN_POINT ( 'NONE',  ( 59.10586122665984732, -20.42344490663941414, 35.00000000000000000 ) ) ;
#7839 = DIRECTION ( 'NONE',  ( -1.000000000000000000, -3.286707217423839940E-17, -2.273843122241288053E-18 ) ) ;
#7840 =( NAMED_UNIT ( * ) SI_UNIT ( $, .STERADIAN. ) SOLID_ANGLE_UNIT ( ) );
#7841 = CARTESIAN_POINT ( 'NONE',  ( 4.767545695837832831, 0.8009384484996263653, 4.000000000000002665 ) ) ;
#7842 = ORIENTED_EDGE ( 'NONE', *, *, #4630, .F. ) ;
#7843 = DIRECTION ( 'NONE',  ( -0.2425356250363330801, 0.9701425001453319874, 0.000000000000000000 ) ) ;
#7844 = ORIENTED_EDGE ( 'NONE', *, *, #6661, .T. ) ;
#7845 = CARTESIAN_POINT ( 'NONE',  ( 20.00000000000000000, 70.00000000000000000, 25.00000000000000000 ) ) ;
#7846 = VERTEX_POINT ( 'NONE', #10772 ) ;
#7847 = ADVANCED_FACE ( 'NONE', ( #10629 ), #12828, .F. ) ;
#7848 = VERTEX_POINT ( 'NONE', #11128 ) ;
#7849 = DIRECTION ( 'NONE',  ( -1.000000000000000000, -1.665334536937734071E-16, 0.000000000000000000 ) ) ;
#7850 = LINE ( 'NONE', #11086, #9863 ) ;
#7851 = CARTESIAN_POINT ( 'NONE',  ( 1.560000000000005826, 0.000000000000000000, 0.000000000000000000 ) ) ;
#7852 = LINE ( 'NONE', #11088, #677 ) ;
#7853 = AXIS2_PLACEMENT_3D ( 'NONE', #1632, #8575, #1787 ) ;
#7854 = SURFACE_STYLE_USAGE ( .BOTH. , #11303 ) ;
#7855 = CARTESIAN_POINT ( 'NONE',  ( 0.000000000000000000, -4.862606272033103139, -3.445885042887453231 ) ) ;
#7856 = SHAPE_REPRESENTATION ( 'connector', ( #11025 ), #1463 ) ;
#7857 = CARTESIAN_POINT ( 'NONE',  ( -2.749999999999997780, 25.49999999999996803, 0.000000000000000000 ) ) ;
#7858 = ADVANCED_FACE ( 'NONE', ( #4426 ), #13287, .T. ) ;
#7859 = DIRECTION ( 'NONE',  ( 1.000000000000000000, 0.000000000000000000, 0.000000000000000000 ) ) ;
#7860 = ORIENTED_EDGE ( 'NONE', *, *, #107, .T. ) ;
#7861 = CARTESIAN_POINT ( 'NONE',  ( 4.960471971868402719, 2.742478347466589028, -3.399327657648797629 ) ) ;
#7862 = CARTESIAN_POINT ( 'NONE',  ( 3.972066048304764507, 3.435565134476452620, 1.180968096049827443 ) ) ;
#7863 = ORIENTED_EDGE ( 'NONE', *, *, #8722, .F. ) ;
#7864 = ORIENTED_EDGE ( 'NONE', *, *, #10732, .T. ) ;
#7865 = ORIENTED_EDGE ( 'NONE', *, *, #11473, .T. ) ;
#7866 = ADVANCED_FACE ( 'NONE', ( #817 ), #12158, .F. ) ;
#7867 = ORIENTED_EDGE ( 'NONE', *, *, #620, .T. ) ;
#7868 = VECTOR ( 'NONE', #7131, 1000.000000000000000 ) ;
#7869 = EDGE_CURVE ( 'NONE', #9332, #5669, #5560, .T. ) ;
#7870 = DIRECTION ( 'NONE',  ( -1.000000000000000000, -3.286707217423839940E-17, -2.273843122241288053E-18 ) ) ;
#7871 = VERTEX_POINT ( 'NONE', #9891 ) ;
#7872 = CARTESIAN_POINT ( 'NONE',  ( 4.030859730899669202, -1.403482646610284323, -3.499999999999992006 ) ) ;
#7873 = DIRECTION ( 'NONE',  ( 0.000000000000000000, -4.440892098500618766E-16, -1.000000000000000000 ) ) ;
#7874 = LINE ( 'NONE', #5732, #4667 ) ;
#7875 = CARTESIAN_POINT ( 'NONE',  ( 31.44014396567294867, 21.68342561534834090, 8.000000000000007105 ) ) ;
#7876 = CARTESIAN_POINT ( 'NONE',  ( 1.560000000000005826, -1.732050807568885631, 0.000000000000000000 ) ) ;
#7877 = ITEM_DEFINED_TRANSFORMATION ( 'NONE', 'NONE', #6387,  #11025 ) ;
#7878 = DIRECTION ( 'NONE',  ( 3.916739600140467622E-15, -1.000000000000000000, -0.000000000000000000 ) ) ;
#7879 = PLANE ( 'NONE',  #5633 ) ;
#7880 = AXIS2_PLACEMENT_3D ( 'NONE', #12542, #12691, #11520 ) ;
#7881 = EDGE_CURVE ( 'NONE', #5390, #12237, #8715, .T. ) ;
#7882 = FACE_BOUND ( 'NONE', #9066, .T. ) ;
#7883 = VERTEX_POINT ( 'NONE', #10030 ) ;
#7884 = ADVANCED_FACE ( 'NONE', ( #5351 ), #13130, .T. ) ;
#7885 = DIRECTION ( 'NONE',  ( 0.000000000000000000, 0.000000000000000000, -1.000000000000000000 ) ) ;
#7886 = ORIENTED_EDGE ( 'NONE', *, *, #479, .F. ) ;
#7887 = VECTOR ( 'NONE', #7243, 1000.000000000000000 ) ;
#7888 = AXIS2_PLACEMENT_3D ( 'NONE', #6898, #11152, #9018 ) ;
#7889 = ORIENTED_EDGE ( 'NONE', *, *, #5332, .F. ) ;
#7890 = AXIS2_PLACEMENT_3D ( 'NONE', #13965, #10877, #2999 ) ;
#7891 = CARTESIAN_POINT ( 'NONE',  ( 4.378301941662550156, -3.528365556573312301, -4.490643565754961486 ) ) ;
#7892 = DIRECTION ( 'NONE',  ( 0.000000000000000000, 0.000000000000000000, -1.000000000000000000 ) ) ;
#7893 =( LENGTH_UNIT ( ) NAMED_UNIT ( * ) SI_UNIT ( .MILLI., .METRE. ) );
#7894 = CARTESIAN_POINT ( 'NONE',  ( 2.000000000000001776, -3.464101615137764156, 0.000000000000000000 ) ) ;
#7895 = B_SPLINE_CURVE_WITH_KNOTS ( 'NONE', 3,
 ( #13511, #10193, #12533, #8956, #10133 ),
 .UNSPECIFIED., .F., .F.,
 ( 4, 1, 4 ),
 ( 0.000000000000000000, 0.002020725942163691807, 0.004041451884327383615 ),
 .UNSPECIFIED. ) ;
#7896 = EDGE_LOOP ( 'NONE', ( #13674, #3545, #4416, #9519 ) ) ;
#7897 = DIRECTION ( 'NONE',  ( 2.168404344970904483E-18, 0.8660254037844375974, -0.5000000000000018874 ) ) ;
#7898 = DIRECTION ( 'NONE',  ( 1.000000000000000000, 1.927470528863118802E-16, 0.000000000000000000 ) ) ;
#7899 = DIRECTION ( 'NONE',  ( 0.000000000000000000, 0.000000000000000000, -1.000000000000000000 ) ) ;
#7900 = CARTESIAN_POINT ( 'NONE',  ( 0.000000000000000000, 5.817072295949927426E-16, -4.750000000000000000 ) ) ;
#7901 = VERTEX_POINT ( 'NONE', #11 ) ;
#7902 = AXIS2_PLACEMENT_3D ( 'NONE', #8542, #3070, #4171 ) ;
#7903 = CARTESIAN_POINT ( 'NONE',  ( 31.38313257588138683, 143.6985259526510674, 25.00000000000000000 ) ) ;
#7904 = ADVANCED_FACE ( 'NONE', ( #5422 ), #14220, .T. ) ;
#7905 = AXIS2_PLACEMENT_3D ( 'NONE', #8816, #3066, #7492 ) ;
#7906 = FACE_OUTER_BOUND ( 'NONE', #9720, .T. ) ;
#7907 = CIRCLE ( 'NONE', #1599, 3.299999999999997158 ) ;
#7908 = ORIENTED_EDGE ( 'NONE', *, *, #6373, .F. ) ;
#7909 = ORIENTED_EDGE ( 'NONE', *, *, #4211, .F. ) ;
#7910 = CARTESIAN_POINT ( 'NONE',  ( 0.000000000000000000, 0.8660254037844428154, 1.500000000000001332 ) ) ;
#7911 = CARTESIAN_POINT ( 'NONE',  ( 31.41872415839353039, 143.5561596226024790, 28.00000000000000000 ) ) ;
#7912 = VECTOR ( 'NONE', #7795, 1000.000000000000000 ) ;
#7913 = CARTESIAN_POINT ( 'NONE',  ( 20.00000000000000000, 47.00000000000000000, -25.00000000000000000 ) ) ;
#7914 = CARTESIAN_POINT ( 'NONE',  ( 0.000000000000000000, 0.000000000000000000, 1.599999999999990319 ) ) ;
#7915 = ORIENTED_EDGE ( 'NONE', *, *, #7032, .F. ) ;
#7916 = DIRECTION ( 'NONE',  ( -0.2425356250363328581, 0.9701425001453318764, 0.000000000000000000 ) ) ;
#7917 = EDGE_CURVE ( 'NONE', #780, #8354, #10709, .T. ) ;
#7918 = ORIENTED_EDGE ( 'NONE', *, *, #4677, .T. ) ;
#7919 = CARTESIAN_POINT ( 'NONE',  ( 0.03458865240850615697, 0.7871057074736870218, 4.000000000000004441 ) ) ;
#7920 = AXIS2_PLACEMENT_3D ( 'NONE', #103, #2712, #9284 ) ;
#7921 = VECTOR ( 'NONE', #5534, 1000.000000000000000 ) ;
#7922 = CARTESIAN_POINT ( 'NONE',  ( 22.00000000000000355, 27.00000000000000355, 25.00000000000000000 ) ) ;
#7923 = CARTESIAN_POINT ( 'NONE',  ( 76.68170757442801744, 39.57655509336063204, -33.00000000000000000 ) ) ;
#7924 = CARTESIAN_POINT ( 'NONE',  ( -3.352586340487487160, -3.837886065734366525, -0.05822226285684464070 ) ) ;
#7925 = CARTESIAN_POINT ( 'NONE',  ( 6.123233995736776143E-16, 199.5765550933606107, -42.00000000000003553 ) ) ;
#7926 = DIRECTION ( 'NONE',  ( 1.000000000000000000, 0.000000000000000000, 0.000000000000000000 ) ) ;
#7927 = CARTESIAN_POINT ( 'NONE',  ( 4.960798468789919369, 2.741591971433226860, 3.400875223032386430 ) ) ;
#7928 = VERTEX_POINT ( 'NONE', #5494 ) ;
#7929 = DIRECTION ( 'NONE',  ( 1.000000000000000000, 0.000000000000000000, 0.000000000000000000 ) ) ;
#7930 = AXIS2_PLACEMENT_3D ( 'NONE', #5261, #14265, #13977 ) ;
#7931 = ORIENTED_EDGE ( 'NONE', *, *, #5101, .T. ) ;
#7932 = CARTESIAN_POINT ( 'NONE',  ( 105.6817075744280174, 109.5765550933605113, 1.102182119232617753E-14 ) ) ;
#7933 = EDGE_CURVE ( 'NONE', #8755, #5025, #9539, .T. ) ;
#7934 = EDGE_CURVE ( 'NONE', #4128, #4481, #6659, .T. ) ;
#7935 = DIRECTION ( 'NONE',  ( -1.000000000000000000, 0.000000000000000000, 0.000000000000000000 ) ) ;
#7936 = ORIENTED_EDGE ( 'NONE', *, *, #9847, .F. ) ;
#7937 = ORIENTED_EDGE ( 'NONE', *, *, #10928, .T. ) ;
#7938 = ORIENTED_EDGE ( 'NONE', *, *, #12246, .T. ) ;
#7939 = AXIS2_PLACEMENT_3D ( 'NONE', #4666, #12621, #8229 ) ;
#7940 = LINE ( 'NONE', #10281, #13198 ) ;
#7941 =( BOUNDED_SURFACE ( )  B_SPLINE_SURFACE ( 3, 2, ( 
 ( #9007, #8185, #6822 ),
 ( #4439, #104, #1263 ),
 ( #8940, #5642, #2227 ),
 ( #7841, #5572, #5908 ),
 ( #2155, #9975, #5979 ),
 ( #6671, #4577, #8864 ) ),
 .UNSPECIFIED., .F., .F., .T. ) 
 B_SPLINE_SURFACE_WITH_KNOTS ( ( 4, 2, 4 ),
 ( 3, 3 ),
 ( 0.01885737098614312032, 0.02120948332636020395, 0.02356159566657728757 ),
 ( 0.000000000000000000, 1.000000000000000000 ),
 .UNSPECIFIED. ) 
 GEOMETRIC_REPRESENTATION_ITEM ( )  RATIONAL_B_SPLINE_SURFACE ( (
 ( 1.000000000000000000, 0.8047781227178442132, 1.000000000000000000),
 ( 1.000000000000000000, 0.8123782226682895180, 1.000000000000000000),
 ( 1.000000000000000000, 0.8190665306020614711, 1.000000000000000000),
 ( 1.000000000000000000, 0.8192358237219363737, 1.000000000000000000),
 ( 1.000000000000000000, 0.8126132530317291547, 1.000000000000000000),
 ( 1.000000000000000000, 0.8047712439471748080, 1.000000000000000000) ) ) 
 REPRESENTATION_ITEM ( '' )  SURFACE ( )  );
#7942 = ORIENTED_EDGE ( 'NONE', *, *, #2729, .F. ) ;
#7943 = DIRECTION ( 'NONE',  ( 0.000000000000000000, 0.000000000000000000, -1.000000000000000000 ) ) ;
#7944 = CARTESIAN_POINT ( 'NONE',  ( 5.000000000000001776, -2.092693589761094763, -4.400105005940151415 ) ) ;
#7945 = DIRECTION ( 'NONE',  ( 0.000000000000000000, 0.000000000000000000, 1.000000000000000000 ) ) ;
#7946 = CARTESIAN_POINT ( 'NONE',  ( 0.000000000000000000, 0.000000000000000000, 2.400000000000013234 ) ) ;
#7947 = DIRECTION ( 'NONE',  ( 0.000000000000000000, 0.000000000000000000, -1.000000000000000000 ) ) ;
#7948 = CONTEXT_DEPENDENT_SHAPE_REPRESENTATION ( #14024, #4740 ) ;
#7949 = CARTESIAN_POINT ( 'NONE',  ( 4.071447262713911996, 2.020725942163681399, 3.499999999999996003 ) ) ;
#7950 = CARTESIAN_POINT ( 'NONE',  ( 6.800000000000028244, -2.309401076758490934, 3.999999999999976019 ) ) ;
#7951 = PRESENTATION_LAYER_ASSIGNMENT (  '', '', ( #14280 ) ) ;
#7952 = VECTOR ( 'NONE', #5434, 1000.000000000000000 ) ;
#7953 = VECTOR ( 'NONE', #14372, 1000.000000000000000 ) ;
#7954 = ORIENTED_EDGE ( 'NONE', *, *, #5206, .T. ) ;
#7955 = CARTESIAN_POINT ( 'NONE',  ( 71.80728622811317052, 38.49793223363091954, 28.00000000000000000 ) ) ;
#7956 = EDGE_LOOP ( 'NONE', ( #169, #4744, #12317, #4733 ) ) ;
#7957 = AXIS2_PLACEMENT_3D ( 'NONE', #10312, #9206, #13768 ) ;
#7958 = ORIENTED_EDGE ( 'NONE', *, *, #8734, .T. ) ;
#7959 = PLANE ( 'NONE',  #1143 ) ;
#7960 = DIRECTION ( 'NONE',  ( -1.000000000000000000, -0.000000000000000000, -0.000000000000000000 ) ) ;
#7961 = CIRCLE ( 'NONE', #10545, 1.500000000000000000 ) ;
#7962 = CYLINDRICAL_SURFACE ( 'NONE', #3778, 3.299999999999976730 ) ;
#7963 = ORIENTED_EDGE ( 'NONE', *, *, #8528, .T. ) ;
#7964 = DIRECTION ( 'NONE',  ( -0.8191520442889913545, 1.003171929053524254E-16, 0.5735764363510468256 ) ) ;
#7965 = DIRECTION ( 'NONE',  ( 1.000000000000000000, -5.046468293750711996E-16, -1.680811587828860421E-31 ) ) ;
#7966 = CARTESIAN_POINT ( 'NONE',  ( 71.80728622811317052, -17.99808865627607801, -25.00000000000000000 ) ) ;
#7967 = ORIENTED_EDGE ( 'NONE', *, *, #10476, .F. ) ;
#7968 = ADVANCED_FACE ( 'NONE', ( #1925 ), #8642, .F. ) ;
#7969 = EDGE_CURVE ( 'NONE', #14130, #1861, #3105, .T. ) ;
#7970 = AXIS2_PLACEMENT_3D ( 'NONE', #297, #11554, #12369 ) ;
#7971 = PRESENTATION_LAYER_ASSIGNMENT (  '', '', ( #8198 ) ) ;
#7972 = VECTOR ( 'NONE', #300, 1000.000000000000000 ) ;
#7973 = DIRECTION ( 'NONE',  ( 0.000000000000000000, 0.000000000000000000, -1.000000000000000000 ) ) ;
#7974 = VERTEX_POINT ( 'NONE', #3241 ) ;
#7975 = ORIENTED_EDGE ( 'NONE', *, *, #1185, .F. ) ;
#7976 = FACE_OUTER_BOUND ( 'NONE', #7321, .T. ) ;
#7977 = FACE_OUTER_BOUND ( 'NONE', #1656, .T. ) ;
#7978 = VECTOR ( 'NONE', #13374, 1000.000000000000000 ) ;
#7979 = ADVANCED_FACE ( 'NONE', ( #10843 ), #10905, .T. ) ;
#7980 = VECTOR ( 'NONE', #1083, 1000.000000000000000 ) ;
#7981 = AXIS2_PLACEMENT_3D ( 'NONE', #828, #3048, #7470 ) ;
#7982 = SURFACE_SIDE_STYLE ('',( #6312 ) ) ;
#7983 = VERTEX_POINT ( 'NONE', #7677 ) ;
#7984 = ORIENTED_EDGE ( 'NONE', *, *, #13048, .T. ) ;
#7985 = FACE_OUTER_BOUND ( 'NONE', #5841, .T. ) ;
#7986 = CARTESIAN_POINT ( 'NONE',  ( 118.6817075744280174, -20.42344490663938927, 33.00000000000002842 ) ) ;
#7987 = DIRECTION ( 'NONE',  ( -4.625929269271486900E-16, -1.000000000000000000, 0.000000000000000000 ) ) ;
#7988 = AXIS2_PLACEMENT_3D ( 'NONE', #7521, #8328, #8490 ) ;
#7989 = VECTOR ( 'NONE', #4413, 1000.000000000000000 ) ;
#7990 = PRODUCT_DEFINITION_SHAPE ( 'NONE', 'NONE',  #14468 ) ;
#7991 = CARTESIAN_POINT ( 'NONE',  ( 28.00000000000000355, 29.99999999999999645, 8.000000000000007105 ) ) ;
#7992 = CARTESIAN_POINT ( 'NONE',  ( 4.988724804725841011, 2.309401076758504701, -4.000000000000003553 ) ) ;
#7993 = EDGE_CURVE ( 'NONE', #433, #3592, #9053, .T. ) ;
#7994 = DIRECTION ( 'NONE',  ( 1.000000000000000000, 0.000000000000000000, 0.000000000000000000 ) ) ;
#7995 = CARTESIAN_POINT ( 'NONE',  ( 4.211140560182201398, 2.431303136016537358, -3.445885042887453231 ) ) ;
#7996 = DIRECTION ( 'NONE',  ( -1.000000000000000000, -0.000000000000000000, -0.000000000000000000 ) ) ;
#7997 = DIRECTION ( 'NONE',  ( 0.000000000000000000, 0.000000000000000000, 1.000000000000000000 ) ) ;
#7998 = AXIS2_PLACEMENT_3D ( 'NONE', #5578, #10122, #1058 ) ;
#7999 = ORIENTED_EDGE ( 'NONE', *, *, #1579, .T. ) ;
#8000 = DIRECTION ( 'NONE',  ( 0.000000000000000000, 0.000000000000000000, 1.000000000000000000 ) ) ;
#8001 = VERTEX_POINT ( 'NONE', #3173 ) ;
#8002 = CARTESIAN_POINT ( 'NONE',  ( 35.00229726637439143, 120.2985749985466839, 25.00000000000000000 ) ) ;
#8003 = ORIENTED_EDGE ( 'NONE', *, *, #9321, .F. ) ;
#8004 = FACE_OUTER_BOUND ( 'NONE', #2962, .T. ) ;
#8005 = ORIENTED_EDGE ( 'NONE', *, *, #1007, .F. ) ;
#8006 = ORIENTED_EDGE ( 'NONE', *, *, #9223, .T. ) ;
#8007 = AXIS2_PLACEMENT_3D ( 'NONE', #8053, #463, #539 ) ;
#8008 = EDGE_LOOP ( 'NONE', ( #9476, #13576, #3355, #14212 ) ) ;
#8009 = DIRECTION ( 'NONE',  ( 1.000000000000000000, 0.000000000000000000, 0.000000000000000000 ) ) ;
#8010 = EDGE_CURVE ( 'NONE', #10506, #1103, #2150, .T. ) ;
#8011 = VERTEX_POINT ( 'NONE', #13341 ) ;
#8012 = CARTESIAN_POINT ( 'NONE',  ( 0.1397371499203132750, 1.362866705341256868, -3.499999999999996891 ) ) ;
#8013 = PRODUCT_DEFINITION ( 'UNKNOWN', '', #14355, #1044 ) ;
#8014 = EDGE_CURVE ( 'NONE', #11907, #1563, #9269, .T. ) ;
#8015 = VECTOR ( 'NONE', #12565, 1000.000000000000000 ) ;
#8016 = LINE ( 'NONE', #3431, #7158 ) ;
#8017 = DIRECTION ( 'NONE',  ( 0.000000000000000000, 0.000000000000000000, -1.000000000000000000 ) ) ;
#8018 = CARTESIAN_POINT ( 'NONE',  ( 22.00000000000000355, 37.00000000000000711, -25.00000000000000000 ) ) ;
#8019 = ORIENTED_EDGE ( 'NONE', *, *, #4531, .T. ) ;
#8020 = DIRECTION ( 'NONE',  ( 0.000000000000000000, 0.000000000000000000, -1.000000000000000000 ) ) ;
#8021 = PRODUCT_DEFINITION_FORMATION_WITH_SPECIFIED_SOURCE ( 'ANY', '', #5648, .NOT_KNOWN. ) ;
#8022 = CARTESIAN_POINT ( 'NONE',  ( 1.647413659512545037, -4.822367972110058965, -0.05822226285685259267 ) ) ;
#8023 = CARTESIAN_POINT ( 'NONE',  ( 1.730488311240535001E-15, 3.268109542640663889, -2.339468227445696158 ) ) ;
#8024 = DIRECTION ( 'NONE',  ( 0.000000000000000000, 0.000000000000000000, 1.000000000000000000 ) ) ;
#8025 = AXIS2_PLACEMENT_3D ( 'NONE', #4599, #57, #13525 ) ;
#8026 = ORIENTED_EDGE ( 'NONE', *, *, #662, .T. ) ;
#8027 = VERTEX_POINT ( 'NONE', #4882 ) ;
#8028 = CARTESIAN_POINT ( 'NONE',  ( -2.749999999999997780, 25.49999999999996803, 8.000000000000007105 ) ) ;
#8029 = ORIENTED_EDGE ( 'NONE', *, *, #5814, .F. ) ;
#8030 = EDGE_LOOP ( 'NONE', ( #4779, #4406, #1370, #2265 ) ) ;
#8031 = LINE ( 'NONE', #2555, #1171 ) ;
#8032 = ADVANCED_FACE ( 'NONE', ( #2777 ), #10439, .F. ) ;
#8033 = DIRECTION ( 'NONE',  ( -1.000000000000000000, -3.286707217423839940E-17, -2.273843122241288053E-18 ) ) ;
#8034 = CARTESIAN_POINT ( 'NONE',  ( -5.000000000000000888, -2.068736481089864743, -4.395493724530259882 ) ) ;
#8035 = DIRECTION ( 'NONE',  ( 0.000000000000000000, 0.000000000000000000, 1.000000000000000000 ) ) ;
#8036 = EDGE_LOOP ( 'NONE', ( #11592, #8533, #9347, #4658 ) ) ;
#8037 = DIRECTION ( 'NONE',  ( 1.000000000000000000, 0.000000000000000000, -0.000000000000000000 ) ) ;
#8038 = SHAPE_REPRESENTATION_RELATIONSHIP ( 'NONE' , 'NONE' ,  #1400, #5565 ) ;
#8039 = AXIS2_PLACEMENT_3D ( 'NONE', #8773, #98, #3301 ) ;
#8040 = CARTESIAN_POINT ( 'NONE',  ( 3.000000000000001332, 4.996003610813205418E-16, 13.31572692736082786 ) ) ;
#8041 = DIRECTION ( 'NONE',  ( 0.000000000000000000, 0.000000000000000000, -1.000000000000000000 ) ) ;
#8042 = ORIENTED_EDGE ( 'NONE', *, *, #13859, .F. ) ;
#8043 = VERTEX_POINT ( 'NONE', #7903 ) ;
#8044 = ADVANCED_FACE ( 'NONE', ( #10376 ), #6117, .T. ) ;
#8045 = CARTESIAN_POINT ( 'NONE',  ( 5.085139881807298146, -2.270820054029154988, 4.066824291575158234 ) ) ;
#8046 = PLANE ( 'NONE',  #5405 ) ;
#8047 = ORIENTED_EDGE ( 'NONE', *, *, #3284, .F. ) ;
#8048 = VERTEX_POINT ( 'NONE', #5631 ) ;
#8049 = DIRECTION ( 'NONE',  ( -1.000000000000000000, -0.000000000000000000, 1.276920294826117846E-16 ) ) ;
#8050 = LINE ( 'NONE', #12462, #7030 ) ;
#8051 = ORIENTED_EDGE ( 'NONE', *, *, #3210, .T. ) ;
#8052 = EDGE_CURVE ( 'NONE', #1916, #11217, #592, .T. ) ;
#8053 = CARTESIAN_POINT ( 'NONE',  ( -118.6817075744281595, 69.57655509336025546, 0.000000000000000000 ) ) ;
#8054 = UNCERTAINTY_MEASURE_WITH_UNIT (LENGTH_MEASURE( 1.000000000000000082E-05 ), #10718, 'distance_accuracy_value', 'NONE');
#8055 = EDGE_CURVE ( 'NONE', #562, #3917, #7066, .T. ) ;
#8056 = DIRECTION ( 'NONE',  ( -1.000000000000000000, 0.000000000000000000, -3.576224061345501491E-16 ) ) ;
#8057 = CARTESIAN_POINT ( 'NONE',  ( 47.12907851819101523, 71.79144999128007498, 25.00000000000000000 ) ) ;
#8058 = ORIENTED_EDGE ( 'NONE', *, *, #10577, .T. ) ;
#8059 = VECTOR ( 'NONE', #10914, 1000.000000000000000 ) ;
#8060 = CARTESIAN_POINT ( 'NONE',  ( 4.175075985190068728, -2.060370777630091244, -3.568666869285586074 ) ) ;
#8061 = PLANE ( 'NONE',  #10645 ) ;
#8062 = CARTESIAN_POINT ( 'NONE',  ( -2.221569714340160529E-16, -4.736529461165888577, -3.381130640444264479 ) ) ;
#8063 = CARTESIAN_POINT ( 'NONE',  ( 0.2117491801717979183, 5.895756138069145003, -4.327903350935045523 ) ) ;
#8064 = CARTESIAN_POINT ( 'NONE',  ( 2.949999999999994404, 0.000000000000000000, 0.000000000000000000 ) ) ;
#8065 = EDGE_CURVE ( 'NONE', #8354, #10068, #1522, .T. ) ;
#8066 = ORIENTED_EDGE ( 'NONE', *, *, #11056, .F. ) ;
#8067 = PLANE ( 'NONE',  #11389 ) ;
#8068 = CARTESIAN_POINT ( 'NONE',  ( 2.836862643238862614, 3.208966885971173078, -3.205052026701826318 ) ) ;
#8069 = ORIENTED_EDGE ( 'NONE', *, *, #1297, .T. ) ;
#8070 = CARTESIAN_POINT ( 'NONE',  ( 5.085009042717535621, -2.271170964606957554, -4.066216496625539634 ) ) ;
#8071 = EDGE_CURVE ( 'NONE', #2483, #4217, #12376, .T. ) ;
#8072 = B_SPLINE_CURVE_WITH_KNOTS ( 'NONE', 3,
 ( #11037, #6565, #5406, #9876, #14346, #5539, #4334, #2116, #9942, #8837, #13317, #3293, #2775, #13689, #1521, #204 ),
 .UNSPECIFIED., .F., .F.,
 ( 4, 3, 3, 3, 3, 4 ),
 ( -2.111273352583301948E-06, 0.000000000000000000, 3.519286887794339423E-05, 7.191842652067419205E-05, 0.0001049868727093471041, 0.0001382836236821663543 ),
 .UNSPECIFIED. ) ;
#8073 = ORIENTED_EDGE ( 'NONE', *, *, #5913, .T. ) ;
#8074 = FACE_OUTER_BOUND ( 'NONE', #10719, .T. ) ;
#8075 = ORIENTED_EDGE ( 'NONE', *, *, #10303, .F. ) ;
#8076 = ORIENTED_EDGE ( 'NONE', *, *, #9517, .F. ) ;
#8077 = PLANE ( 'NONE',  #10138 ) ;
#8078 = PLANE ( 'NONE',  #4279 ) ;
#8079 = EDGE_CURVE ( 'NONE', #11217, #698, #4089, .T. ) ;
#8080 = ORIENTED_EDGE ( 'NONE', *, *, #12872, .F. ) ;
#8081 = CARTESIAN_POINT ( 'NONE',  ( 1.560000000000005826, 0.8660254037844428154, -1.500000000000001332 ) ) ;
#8082 = LINE ( 'NONE', #4741, #6499 ) ;
#8083 = CARTESIAN_POINT ( 'NONE',  ( 28.00000000000000355, 35.49999999999997868, 8.000000000000007105 ) ) ;
#8084 = DIRECTION ( 'NONE',  ( 1.000000000000000000, 4.625929269271485914E-16, 0.000000000000000000 ) ) ;
#8085 = LINE ( 'NONE', #4609, #10773 ) ;
#8086 = CARTESIAN_POINT ( 'NONE',  ( -2.750000000000003997, 40.49999999999999289, 0.000000000000000000 ) ) ;
#8087 = DIRECTION ( 'NONE',  ( 0.000000000000000000, 0.000000000000000000, -1.000000000000000000 ) ) ;
#8088 = AXIS2_PLACEMENT_3D ( 'NONE', #5433, #12166, #9901 ) ;
#8089 = APPLICATION_CONTEXT ( 'automotive_design' ) ;
#8090 = ORIENTED_EDGE ( 'NONE', *, *, #2268, .F. ) ;
#8091 = EDGE_CURVE ( 'NONE', #6826, #1257, #7139, .T. ) ;
#8092 = ORIENTED_EDGE ( 'NONE', *, *, #10125, .T. ) ;
#8093 = CIRCLE ( 'NONE', #6896, 5.000000000000004441 ) ;
#8094 = ORIENTED_EDGE ( 'NONE', *, *, #1727, .T. ) ;
#8095 = LINE ( 'NONE', #2334, #7345 ) ;
#8096 = EDGE_LOOP ( 'NONE', ( #7591, #12982, #78, #6690 ) ) ;
#8097 = VERTEX_POINT ( 'NONE', #1669 ) ;
#8098 = CARTESIAN_POINT ( 'NONE',  ( 76.68170757442796059, 3.003422806631532356E-13, -33.00000000000000000 ) ) ;
#8099 = CARTESIAN_POINT ( 'NONE',  ( 4.197393957002307552, 7.823395958202418729E-14, -3.203767560748914445 ) ) ;
#8100 = CARTESIAN_POINT ( 'NONE',  ( -5.000000000000000000, 2.119023573395804050, -4.142091658825685307 ) ) ;
#8101 = DIRECTION ( 'NONE',  ( -0.2425356250363329969, 0.9701425001453318764, -9.251858538542973800E-15 ) ) ;
#8102 = AXIS2_PLACEMENT_3D ( 'NONE', #2456, #6907, #11373 ) ;
#8103 = DIRECTION ( 'NONE',  ( 0.000000000000000000, 0.000000000000000000, -1.000000000000000000 ) ) ;
#8104 = CARTESIAN_POINT ( 'NONE',  ( -99.68170757442806007, 109.5765550933605113, -8.165854576837898311E-15 ) ) ;
#8105 = CARTESIAN_POINT ( 'NONE',  ( -1.387778780781445676E-14, -4.618802153517016507, -0.5000000000000004441 ) ) ;
#8106 = VERTEX_POINT ( 'NONE', #6040 ) ;
#8107 = ADVANCED_FACE ( 'NONE', ( #8997 ), #3457, .T. ) ;
#8108 = EDGE_CURVE ( 'NONE', #1573, #12192, #13903, .T. ) ;
#8109 = CARTESIAN_POINT ( 'NONE',  ( 20.00000000000000355, 50.00000000000000000, 25.00000000000000000 ) ) ;
#8110 = VECTOR ( 'NONE', #8660, 1000.000000000000000 ) ;
#8111 = AXIS2_PLACEMENT_3D ( 'NONE', #8832, #6559, #3371 ) ;
#8112 = EDGE_LOOP ( 'NONE', ( #1052, #6190, #2295, #127 ) ) ;
#8113 = EDGE_CURVE ( 'NONE', #6870, #10194, #11631, .T. ) ;
#8114 = CARTESIAN_POINT ( 'NONE',  ( 6.202806007537712125E-14, -5.987311224403027765, -4.630826434870603414 ) ) ;
#8115 = CARTESIAN_POINT ( 'NONE',  ( 22.00000000000000711, 17.00000000000000000, 25.00000000000000000 ) ) ;
#8116 = VECTOR ( 'NONE', #1995, 1000.000000000000000 ) ;
#8117 = VECTOR ( 'NONE', #4721, 1000.000000000000000 ) ;
#8118 = ORIENTED_EDGE ( 'NONE', *, *, #382, .T. ) ;
#8119 = ORIENTED_EDGE ( 'NONE', *, *, #10174, .F. ) ;
#8120 = CARTESIAN_POINT ( 'NONE',  ( -118.6817075744279748, -20.42344490663959178, 33.00000000000002842 ) ) ;
#8121 = EDGE_CURVE ( 'NONE', #6929, #7126, #2289, .T. ) ;
#8122 = CARTESIAN_POINT ( 'NONE',  ( 5.098157279263967112, 2.347014727359150843, -4.065148753898843559 ) ) ;
#8123 = EDGE_CURVE ( 'NONE', #11544, #1594, #8605, .T. ) ;
#8124 = ORIENTED_EDGE ( 'NONE', *, *, #10032, .T. ) ;
#8125 = CARTESIAN_POINT ( 'NONE',  ( 12.50000000000002132, 12.49999999999999289, 25.00000000000000000 ) ) ;
#8126 = ORIENTED_EDGE ( 'NONE', *, *, #13347, .F. ) ;
#8127 = ORIENTED_EDGE ( 'NONE', *, *, #12008, .F. ) ;
#8128 = AXIS2_PLACEMENT_3D ( 'NONE', #5662, #2098, #12980 ) ;
#8129 = CARTESIAN_POINT ( 'NONE',  ( -0.3208286057739688779, 4.433571671609684017, -0.3503314178412602620 ) ) ;
#8130 = CARTESIAN_POINT ( 'NONE',  ( 4.871660775260041376, -3.136983646853262808, 2.711317785102830502 ) ) ;
#8131 = ORIENTED_EDGE ( 'NONE', *, *, #10025, .F. ) ;
#8132 = DIRECTION ( 'NONE',  ( 0.000000000000000000, 0.000000000000000000, -1.000000000000000000 ) ) ;
#8133 = DIRECTION ( 'NONE',  ( 1.000000000000000000, 0.000000000000000000, 0.000000000000000000 ) ) ;
#8134 =( NAMED_UNIT ( * ) SI_UNIT ( $, .STERADIAN. ) SOLID_ANGLE_UNIT ( ) );
#8135 = DIRECTION ( 'NONE',  ( -1.000000000000000000, 0.000000000000000000, 0.000000000000000000 ) ) ;
#8136 = EDGE_CURVE ( 'NONE', #10931, #4994, #9462, .T. ) ;
#8137 = CYLINDRICAL_SURFACE ( 'NONE', #4282, 3.299999999999976730 ) ;
#8138 = ORIENTED_EDGE ( 'NONE', *, *, #936, .F. ) ;
#8139 = PLANE ( 'NONE',  #1668 ) ;
#8140 = LINE ( 'NONE', #13515, #14014 ) ;
#8141 = CARTESIAN_POINT ( 'NONE',  ( 4.686019787951550164, -3.464101615137729517, 2.000000000000000444 ) ) ;
#8142 = EDGE_CURVE ( 'NONE', #10034, #11932, #10473, .T. ) ;
#8143 = ORIENTED_EDGE ( 'NONE', *, *, #12577, .F. ) ;
#8144 = CARTESIAN_POINT ( 'NONE',  ( 3.511755186886754476, -2.826662030176371410, -3.297382984111599580 ) ) ;
#8145 = EDGE_CURVE ( 'NONE', #13288, #14042, #6497, .T. ) ;
#8146 = CARTESIAN_POINT ( 'NONE',  ( -3.999999999999982681, -8.023096076392732812E-15, -2.842992957459206771 ) ) ;
#8147 = VECTOR ( 'NONE', #5044, 1000.000000000000000 ) ;
#8148 = ORIENTED_EDGE ( 'NONE', *, *, #11559, .F. ) ;
#8149 = CARTESIAN_POINT ( 'NONE',  ( 20.00000000000000000, 60.00000000000000711, 25.00000000000000000 ) ) ;
#8150 = ORIENTED_EDGE ( 'NONE', *, *, #7391, .F. ) ;
#8151 = EDGE_LOOP ( 'NONE', ( #2630, #6432, #8006, #1940 ) ) ;
#8152 = DIRECTION ( 'NONE',  ( 0.2425356250363327748, -0.9701425001453319874, -0.000000000000000000 ) ) ;
#8153 = DIRECTION ( 'NONE',  ( -1.000000000000000000, 0.000000000000000000, -2.081668171172169499E-16 ) ) ;
#8154 = ORIENTED_EDGE ( 'NONE', *, *, #13134, .F. ) ;
#8155 = PLANE ( 'NONE',  #9816 ) ;
#8156 = VECTOR ( 'NONE', #10152, 1000.000000000000000 ) ;
#8157 = CARTESIAN_POINT ( 'NONE',  ( 4.872112557124452792, 0.7838640816431967639, 4.072377784234222808 ) ) ;
#8158 = FILL_AREA_STYLE ('',( #275 ) ) ;
#8159 = EDGE_CURVE ( 'NONE', #11202, #7559, #9277, .T. ) ;
#8160 = FACE_BOUND ( 'NONE', #7723, .T. ) ;
#8161 = FACE_OUTER_BOUND ( 'NONE', #12344, .T. ) ;
#8162 = COLOUR_RGB ( '', 0.66274510, 0.83137255, 0.94901961) ;
#8163 = CONTEXT_DEPENDENT_SHAPE_REPRESENTATION ( #1771, #4069 ) ;
#8164 = DIRECTION ( 'NONE',  ( -2.081668171172168760E-16, 0.000000000000000000, -1.000000000000000000 ) ) ;
#8165 = LINE ( 'NONE', #498, #7639 ) ;
#8166 = PLANE ( 'NONE',  #8465 ) ;
#8167 = DIRECTION ( 'NONE',  ( 0.000000000000000000, 0.000000000000000000, 1.000000000000000000 ) ) ;
#8168 = AXIS2_PLACEMENT_3D ( 'NONE', #10749, #12064, #11850 ) ;
#8169 = ORIENTED_EDGE ( 'NONE', *, *, #2294, .T. ) ;
#8170 = CARTESIAN_POINT ( 'NONE',  ( 4.154306624730762287, 2.398490048085581083, -3.421999068284434120 ) ) ;
#8171 = ORIENTED_EDGE ( 'NONE', *, *, #381, .T. ) ;
#8172 = ORIENTED_EDGE ( 'NONE', *, *, #928, .T. ) ;
#8173 = PLANE ( 'NONE',  #4464 ) ;
#8174 = CARTESIAN_POINT ( 'NONE',  ( 27.57694101601105530, 130.0000000000000000, 25.00000000000000000 ) ) ;
#8175 = CARTESIAN_POINT ( 'NONE',  ( -5.000000000000000888, -1.027005139385383847, -4.269881284526090504 ) ) ;
#8176 = LINE ( 'NONE', #11622, #9085 ) ;
#8177 = ADVANCED_FACE ( 'NONE', ( #9500 ), #6201, .F. ) ;
#8178 = CARTESIAN_POINT ( 'NONE',  ( 30.15499999999998693, 1.387778780781445182E-16, 2.499999999999999112 ) ) ;
#8179 = COLOUR_RGB ( '', 0.40784314, 0.44705882, 0.49803922) ;
#8180 = ORIENTED_EDGE ( 'NONE', *, *, #2312, .F. ) ;
#8181 = ADVANCED_BREP_SHAPE_REPRESENTATION ( '', ( #11715, #11025 ), #6837 ) ;
#8182 = CIRCLE ( 'NONE', #7472, 9.000000000000005329 ) ;
#8183 = DIRECTION ( 'NONE',  ( 1.734723475976770502E-18, -4.440892098500621231E-16, -1.000000000000000000 ) ) ;
#8184 = DIRECTION ( 'NONE',  ( -1.000000000000000000, 0.000000000000000000, 0.000000000000000000 ) ) ;
#8185 = CARTESIAN_POINT ( 'NONE',  ( 5.085008806763689826, -2.385860035267069357, 4.000000000000003553 ) ) ;
#8186 = CARTESIAN_POINT ( 'NONE',  ( 18.68170757442808849, 141.2731697022877313, -35.00000000000000000 ) ) ;
#8187 = ADVANCED_FACE ( 'NONE', ( #10741 ), #2933, .T. ) ;
#8188 = CARTESIAN_POINT ( 'NONE',  ( 20.00000000000000000, 27.00000000000000355, 25.00000000000000000 ) ) ;
#8189 = ORIENTED_EDGE ( 'NONE', *, *, #9847, .T. ) ;
#8190 = CIRCLE ( 'NONE', #13356, 300.0000000000001137 ) ;
#8191 = ORIENTED_EDGE ( 'NONE', *, *, #3251, .F. ) ;
#8192 = CARTESIAN_POINT ( 'NONE',  ( 22.00000000000000355, 47.00000000000000000, 25.00000000000000000 ) ) ;
#8193 = CARTESIAN_POINT ( 'NONE',  ( 71.80728622811317052, -17.99808865627607801, -28.00000000000000000 ) ) ;
#8194 = ADVANCED_FACE ( 'NONE', ( #13170 ), #793, .T. ) ;
#8195 = EDGE_CURVE ( 'NONE', #7236, #549, #6017, .T. ) ;
#8196 = SURFACE_SIDE_STYLE ('',( #5921 ) ) ;
#8197 = AXIS2_PLACEMENT_3D ( 'NONE', #1532, #2417, #11477 ) ;
#8198 = STYLED_ITEM ( 'NONE', ( #2654 ), #2974 ) ;
#8199 = VECTOR ( 'NONE', #13989, 1000.000000000000114 ) ;
#8200 = EDGE_LOOP ( 'NONE', ( #10266, #1567 ) ) ;
#8201 = CARTESIAN_POINT ( 'NONE',  ( -108.6817075744280316, -30.42344490663958112, -32.00000000000002842 ) ) ;
#8202 = CARTESIAN_POINT ( 'NONE',  ( 5.024612689793150899, 2.312654742478270631, -4.005635514337496872 ) ) ;
#8203 = EDGE_LOOP ( 'NONE', ( #3461, #3239, #5407 ) ) ;
#8204 = CARTESIAN_POINT ( 'NONE',  ( 28.00000000000000355, 29.99999999999999645, -6.999999999999992006 ) ) ;
#8205 = AXIS2_PLACEMENT_3D ( 'NONE', #1877, #710, #4231 ) ;
#8206 = VECTOR ( 'NONE', #12629, 1000.000000000000000 ) ;
#8207 = CARTESIAN_POINT ( 'NONE',  ( 0.000000000000000000, 4.618802153517016507, -0.5000000000000004441 ) ) ;
#8208 = DIRECTION ( 'NONE',  ( 0.000000000000000000, 1.000000000000000000, -0.000000000000000000 ) ) ;
#8209 = FACE_OUTER_BOUND ( 'NONE', #1970, .T. ) ;
#8210 = FACE_OUTER_BOUND ( 'NONE', #340, .T. ) ;
#8211 = SURFACE_STYLE_FILL_AREA ( #13797 ) ;
#8212 = CARTESIAN_POINT ( 'NONE',  ( 4.296971609537894032, 3.292644976429773163, -4.396693167834091476 ) ) ;
#8213 = CARTESIAN_POINT ( 'NONE',  ( -6.938893903907228378E-15, 24.50000000000002132, 8.000000000000007105 ) ) ;
#8214 = VERTEX_POINT ( 'NONE', #8608 ) ;
#8215 = DIRECTION ( 'NONE',  ( -1.000000000000000000, 0.000000000000000000, 0.000000000000000000 ) ) ;
#8216 = CARTESIAN_POINT ( 'NONE',  ( -2.750000000000003553, 40.49999999999999289, 0.000000000000000000 ) ) ;
#8217 =( GEOMETRIC_REPRESENTATION_CONTEXT ( 3 ) GLOBAL_UNCERTAINTY_ASSIGNED_CONTEXT ( ( #4138 ) ) GLOBAL_UNIT_ASSIGNED_CONTEXT ( ( #5511, #6676, #10132 ) ) REPRESENTATION_CONTEXT ( 'NONE', 'WORKASPACE' ) );
#8218 = AXIS2_PLACEMENT_3D ( 'NONE', #8423, #881, #5059 ) ;
#8219 = CARTESIAN_POINT ( 'NONE',  ( 4.175003227304316944, 2.208362916365297135, -3.169254239516197114 ) ) ;
#8220 = ORIENTED_EDGE ( 'NONE', *, *, #11206, .F. ) ;
#8221 = DIRECTION ( 'NONE',  ( 0.000000000000000000, 1.000000000000000000, 0.000000000000000000 ) ) ;
#8222 = DIRECTION ( 'NONE',  ( 1.000000000000000000, 0.000000000000000000, 0.000000000000000000 ) ) ;
#8223 = PLANE ( 'NONE',  #1414 ) ;
#8224 = ORIENTED_EDGE ( 'NONE', *, *, #4462, .T. ) ;
#8225 = ORIENTED_EDGE ( 'NONE', *, *, #409, .T. ) ;
#8226 = DIRECTION ( 'NONE',  ( 1.000000000000000000, 0.000000000000000000, -0.000000000000000000 ) ) ;
#8227 = LINE ( 'NONE', #1655, #11731 ) ;
#8228 = VERTEX_POINT ( 'NONE', #655 ) ;
#8229 = DIRECTION ( 'NONE',  ( 1.000000000000000000, 0.000000000000000000, 0.000000000000000000 ) ) ;
#8230 = VECTOR ( 'NONE', #4819, 1000.000000000000000 ) ;
#8231 = ADVANCED_FACE ( 'NONE', ( #7498 ), #3479, .T. ) ;
#8232 = PRODUCT ( 'MirrorHardened Serrated Safety Wedge', 'MirrorHardened Serrated Safety Wedge', '', ( #7311 ) ) ;
#8233 = DIRECTION ( 'NONE',  ( -0.000000000000000000, -0.000000000000000000, -1.000000000000000000 ) ) ;
#8234 =( NAMED_UNIT ( * ) PLANE_ANGLE_UNIT ( ) SI_UNIT ( $, .RADIAN. ) );
#8235 = CARTESIAN_POINT ( 'NONE',  ( 8.000000000000000000, 25.49999999999996803, 0.000000000000000000 ) ) ;
#8236 = CARTESIAN_POINT ( 'NONE',  ( 39.77836601746437850, 91.19429999418670718, 25.00000000000000000 ) ) ;
#8237 = ITEM_DEFINED_TRANSFORMATION ( 'NONE', 'NONE', #10842,  #11025 ) ;
#8238 = FACE_OUTER_BOUND ( 'NONE', #903, .T. ) ;
#8239 = CARTESIAN_POINT ( 'NONE',  ( 0.000000000000000000, 3.031088913245536087, -1.750000000000001554 ) ) ;
#8240 = CARTESIAN_POINT ( 'NONE',  ( 13.00000000000000355, 24.50000000000001421, 8.000000000000007105 ) ) ;
#8241 = DIRECTION ( 'NONE',  ( 1.000000000000000000, 1.723842398015259277E-15, -0.000000000000000000 ) ) ;
#8242 = EDGE_CURVE ( 'NONE', #9976, #14165, #10878, .T. ) ;
#8243 = EDGE_LOOP ( 'NONE', ( #4050, #56, #400 ) ) ;
#8244 = CIRCLE ( 'NONE', #1964, 3.000000000000003553 ) ;
#8245 = LINE ( 'NONE', #12791, #4540 ) ;
#8246 = ORIENTED_EDGE ( 'NONE', *, *, #4991, .T. ) ;
#8247 = ORIENTED_EDGE ( 'NONE', *, *, #4663, .F. ) ;
#8248 = DIRECTION ( 'NONE',  ( -2.273843122241288438E-18, -5.551115123125783935E-17, -1.000000000000000000 ) ) ;
#8249 = ADVANCED_FACE ( 'NONE', ( #7574 ), #14052, .T. ) ;
#8250 = CARTESIAN_POINT ( 'NONE',  ( -1.144235203016676250, -3.958177651039096911, -0.09382832055446391206 ) ) ;
#8251 = DIRECTION ( 'NONE',  ( -2.732679788978644593E-17, -0.8660254037844379305, 0.5000000000000013323 ) ) ;
#8252 = CARTESIAN_POINT ( 'NONE',  ( 76.68170757442801744, 29.57655509336063204, -33.00000000000000000 ) ) ;
#8253 = LINE ( 'NONE', #13495, #4886 ) ;
#8254 = CARTESIAN_POINT ( 'NONE',  ( 42.27836601746437850, 91.19429999418670718, 25.00000000000000000 ) ) ;
#8255 = LINE ( 'NONE', #12727, #11710 ) ;
#8256 = DIRECTION ( 'NONE',  ( 0.000000000000000000, 0.000000000000000000, 1.000000000000000000 ) ) ;
#8257 = CARTESIAN_POINT ( 'NONE',  ( 1.391697335622811948, 4.043246145443379014, -3.203898532754351436 ) ) ;
#8258 = DIRECTION ( 'NONE',  ( -1.734723475976770694E-18, 4.440892098500621231E-16, 1.000000000000000000 ) ) ;
#8259 = AXIS2_PLACEMENT_3D ( 'NONE', #9257, #12618, #490 ) ;
#8260 = LINE ( 'NONE', #9214, #3341 ) ;
#8261 = VERTEX_POINT ( 'NONE', #2026 ) ;
#8262 = EDGE_CURVE ( 'NONE', #9023, #13190, #13686, .T. ) ;
#8263 = EDGE_LOOP ( 'NONE', ( #3658, #10324 ) ) ;
#8264 = VERTEX_POINT ( 'NONE', #11913 ) ;
#8265 = CARTESIAN_POINT ( 'NONE',  ( -3.680118525130247953, 2.494084732383337055, -0.3507732604232524642 ) ) ;
#8266 = DIRECTION ( 'NONE',  ( -1.000000000000000000, 0.000000000000000000, 0.000000000000000000 ) ) ;
#8267 = EDGE_LOOP ( 'NONE', ( #2826, #8612, #4193, #7217 ) ) ;
#8268 = ORIENTED_EDGE ( 'NONE', *, *, #3496, .T. ) ;
#8269 = CARTESIAN_POINT ( 'NONE',  ( 22.00000000000000355, 27.00000000000000355, 25.00000000000000000 ) ) ;
#8270 = CARTESIAN_POINT ( 'NONE',  ( -5.170224855064537550, -2.788471980053867760, -4.589066185948674104 ) ) ;
#8271 = ORIENTED_EDGE ( 'NONE', *, *, #11035, .F. ) ;
#8272 = CLOSED_SHELL ( 'NONE', ( #12286, #5120, #2099, #14416, #1454, #3404, #6321, #12139, #9075, #14005, #4764, #11165, #7661, #6922, #4478, #1960, #5278, #6115, #7756, #3106, #12698, #10882, #9234, #4170, #8416, #10069, #5150, #13635, #2989 ) ) ;
#8273 = EDGE_CURVE ( 'NONE', #13731, #1368, #9574, .T. ) ;
#8274 = CARTESIAN_POINT ( 'NONE',  ( 108.6817075744280743, 124.5765550933606107, 25.00000000000000000 ) ) ;
#8275 = ORIENTED_EDGE ( 'NONE', *, *, #11562, .F. ) ;
#8276 = ADVANCED_FACE ( 'NONE', ( #4022 ), #1806, .F. ) ;
#8277 = CARTESIAN_POINT ( 'NONE',  ( 20.00000000000000000, 27.00000000000000355, -25.00000000000000000 ) ) ;
#8278 = CARTESIAN_POINT ( 'NONE',  ( 4.071447262713911996, 2.020725942163681399, 3.499999999999996003 ) ) ;
#8279 = DIRECTION ( 'NONE',  ( 0.000000000000000000, 0.000000000000000000, 1.000000000000000000 ) ) ;
#8280 = ORIENTED_EDGE ( 'NONE', *, *, #1445, .T. ) ;
#8281 = CYLINDRICAL_SURFACE ( 'NONE', #5155, 2.600000000000004974 ) ;
#8282 = DIRECTION ( 'NONE',  ( 1.734723475976770502E-18, -4.440892098500621231E-16, -1.000000000000000000 ) ) ;
#8283 = ORIENTED_EDGE ( 'NONE', *, *, #3260, .F. ) ;
#8284 = FACE_OUTER_BOUND ( 'NONE', #8798, .T. ) ;
#8285 = FACE_OUTER_BOUND ( 'NONE', #11648, .T. ) ;
#8286 = ORIENTED_EDGE ( 'NONE', *, *, #12246, .F. ) ;
#8287 = PRESENTATION_STYLE_ASSIGNMENT (( #4148 ) ) ;
#8288 = ORIENTED_EDGE ( 'NONE', *, *, #4108, .T. ) ;
#8289 = DIRECTION ( 'NONE',  ( -0.000000000000000000, -0.000000000000000000, -1.000000000000000000 ) ) ;
#8290 = DIRECTION ( 'NONE',  ( 0.000000000000000000, 0.000000000000000000, 1.000000000000000000 ) ) ;
#8291 = EDGE_LOOP ( 'NONE', ( #538, #13836, #5529, #14320 ) ) ;
#8292 = DIRECTION ( 'NONE',  ( -1.000000000000000000, 0.000000000000000000, 0.000000000000000000 ) ) ;
#8293 = FACE_BOUND ( 'NONE', #6888, .T. ) ;
#8294 = CARTESIAN_POINT ( 'NONE',  ( 5.103279350327411201, 4.707503328691851507, -2.309077599722808952E-14 ) ) ;
#8295 = EDGE_LOOP ( 'NONE', ( #3967, #4767, #6180, #329 ) ) ;
#8296 = ORIENTED_EDGE ( 'NONE', *, *, #3707, .T. ) ;
#8297 = CARTESIAN_POINT ( 'NONE',  ( 59.10586122665984732, -20.42344490663941414, 35.00000000000000000 ) ) ;
#8298 = CARTESIAN_POINT ( 'NONE',  ( 28.00000000000000355, 29.99999999999999645, -24.99999999999999289 ) ) ;
#8299 = ORIENTED_EDGE ( 'NONE', *, *, #14217, .F. ) ;
#8300 = DIRECTION ( 'NONE',  ( 1.000000000000000000, 0.000000000000000000, 0.000000000000000000 ) ) ;
#8301 = LINE ( 'NONE', #5092, #866 ) ;
#8302 =( NAMED_UNIT ( * ) SI_UNIT ( $, .STERADIAN. ) SOLID_ANGLE_UNIT ( ) );
#8303 = CARTESIAN_POINT ( 'NONE',  ( 30.60000000000001563, 1.451737380178518264E-16, -2.055000000000000160 ) ) ;
#8304 = CARTESIAN_POINT ( 'NONE',  ( 22.00000000000000711, 20.00000000000000355, -25.00000000000000000 ) ) ;
#8305 = DIRECTION ( 'NONE',  ( 0.000000000000000000, 0.000000000000000000, -1.000000000000000000 ) ) ;
#8306 = CARTESIAN_POINT ( 'NONE',  ( 0.000000000000000000, 0.000000000000000000, 0.000000000000000000 ) ) ;
#8307 = DIRECTION ( 'NONE',  ( 1.000000000000000000, 0.000000000000000000, 0.000000000000000000 ) ) ;
#8308 = CARTESIAN_POINT ( 'NONE',  ( -1.432312439535613269, -4.946556719366752120, -0.1121614189353486168 ) ) ;
#8309 = ADVANCED_FACE ( 'NONE', ( #9856 ), #8819, .T. ) ;
#8310 = EDGE_CURVE ( 'NONE', #10136, #47, #2783, .T. ) ;
#8311 = ORIENTED_EDGE ( 'NONE', *, *, #7000, .T. ) ;
#8312 = DIRECTION ( 'NONE',  ( 1.734723475976807094E-16, -0.000000000000000000, 1.000000000000000000 ) ) ;
#8313 = ORIENTED_EDGE ( 'NONE', *, *, #13289, .F. ) ;
#8314 = VERTEX_POINT ( 'NONE', #11018 ) ;
#8315 = EDGE_CURVE ( 'NONE', #6118, #2918, #12546, .T. ) ;
#8316 = DIRECTION ( 'NONE',  ( 1.000000000000000000, 0.000000000000000000, 0.000000000000000000 ) ) ;
#8317 = CARTESIAN_POINT ( 'NONE',  ( -3.999999999999996447, 1.563622288139188354, -0.2253451193528278329 ) ) ;
#8318 = CARTESIAN_POINT ( 'NONE',  ( -108.6817075744279748, -20.42344490663957046, 33.00000000000002842 ) ) ;
#8319 = DIRECTION ( 'NONE',  ( -1.000000000000000000, 0.000000000000000000, 0.000000000000000000 ) ) ;
#8320 = LINE ( 'NONE', #2791, #13370 ) ;
#8321 = DIRECTION ( 'NONE',  ( 0.000000000000000000, 8.482162385747133845E-47, -1.000000000000000000 ) ) ;
#8322 = DIRECTION ( 'NONE',  ( -1.000000000000000000, -5.046468293750711996E-16, -1.680811587828860421E-31 ) ) ;
#8323 = EDGE_CURVE ( 'NONE', #11470, #1840, #11160, .T. ) ;
#8324 = CARTESIAN_POINT ( 'NONE',  ( -28.00000000000000355, 29.99999999999999645, 0.000000000000000000 ) ) ;
#8325 =( BOUNDED_SURFACE ( )  B_SPLINE_SURFACE ( 3, 2, ( 
 ( #3802, #10221, #4674 ),
 ( #10374, #5962, #203 ),
 ( #10518, #2698, #2472 ),
 ( #10436, #7137, #424 ),
 ( #13615, #4811, #6038 ),
 ( #11462, #13900, #10291 ) ),
 .UNSPECIFIED., .F., .F., .T. ) 
 B_SPLINE_SURFACE_WITH_KNOTS ( ( 4, 2, 4 ),
 ( 3, 3 ),
 ( 0.02018906359535397113, 0.02264947622839650482, 0.02510988886143903503 ),
 ( 0.000000000000000000, 1.000000000000000000 ),
 .UNSPECIFIED. ) 
 GEOMETRIC_REPRESENTATION_ITEM ( )  RATIONAL_B_SPLINE_SURFACE ( (
 ( 1.000000000000000000, 0.8047781357041526862, 1.000000000000000000),
 ( 1.000000000000000000, 0.8123775905861532198, 1.000000000000000000),
 ( 1.000000000000000000, 0.8190671519372876297, 1.000000000000000000),
 ( 1.000000000000000000, 0.8192352278312100555, 1.000000000000000000),
 ( 1.000000000000000000, 0.8126131206996278777, 1.000000000000000000),
 ( 1.000000000000000000, 0.8047712494894333490, 1.000000000000000000) ) ) 
 REPRESENTATION_ITEM ( '' )  SURFACE ( )  );
#8326 = EDGE_CURVE ( 'NONE', #10731, #3034, #9929, .T. ) ;
#8327 = CARTESIAN_POINT ( 'NONE',  ( -140.0000000000003411, 199.5765550933606107, 47.99999999999998579 ) ) ;
#8328 = DIRECTION ( 'NONE',  ( -0.000000000000000000, -0.000000000000000000, -1.000000000000000000 ) ) ;
#8329 = EDGE_CURVE ( 'NONE', #4731, #6928, #6622, .T. ) ;
#8330 = ORIENTED_EDGE ( 'NONE', *, *, #5851, .T. ) ;
#8331 = EDGE_CURVE ( 'NONE', #12327, #11314, #7721, .T. ) ;
#8332 = ORIENTED_EDGE ( 'NONE', *, *, #12577, .T. ) ;
#8333 = VERTEX_POINT ( 'NONE', #11093 ) ;
#8334 = VECTOR ( 'NONE', #7701, 1000.000000000000000 ) ;
#8335 = PLANE ( 'NONE',  #4057 ) ;
#8336 = DIRECTION ( 'NONE',  ( -1.000000000000000000, -0.000000000000000000, -0.000000000000000000 ) ) ;
#8337 = EDGE_CURVE ( 'NONE', #5102, #5269, #2314, .T. ) ;
#8338 = ADVANCED_FACE ( 'NONE', ( #14401 ), #8965, .F. ) ;
#8339 = ORIENTED_EDGE ( 'NONE', *, *, #12442, .F. ) ;
#8340 = VECTOR ( 'NONE', #12105, 1000.000000000000000 ) ;
#8341 = FACE_OUTER_BOUND ( 'NONE', #12735, .T. ) ;
#8342 = AXIS2_PLACEMENT_3D ( 'NONE', #11770, #9572, #14051 ) ;
#8343 = LINE ( 'NONE', #753, #13620 ) ;
#8344 = ORIENTED_EDGE ( 'NONE', *, *, #10257, .F. ) ;
#8345 = ADVANCED_FACE ( 'NONE', ( #13233 ), #1069, .F. ) ;
#8346 = DIRECTION ( 'NONE',  ( 0.000000000000000000, 0.000000000000000000, 1.000000000000000000 ) ) ;
#8347 = EDGE_CURVE ( 'NONE', #7126, #12483, #11150, .T. ) ;
#8348 = PRODUCT_DEFINITION_SHAPE ( 'NONE', 'NONE',  #9274 ) ;
#8349 = ORIENTED_EDGE ( 'NONE', *, *, #13491, .T. ) ;
#8350 = CARTESIAN_POINT ( 'NONE',  ( 21.68170757442808849, 141.2731697022877313, 23.00000000000000000 ) ) ;
#8351 = CARTESIAN_POINT ( 'NONE',  ( 36.31750732272606541, 144.5765550933605823, -199.4258611313499330 ) ) ;
#8352 = CARTESIAN_POINT ( 'NONE',  ( 22.00000000000000000, 57.00000000000000000, 25.00000000000000000 ) ) ;
#8353 = VECTOR ( 'NONE', #2656, 1000.000000000000000 ) ;
#8354 = VERTEX_POINT ( 'NONE', #12411 ) ;
#8355 = CIRCLE ( 'NONE', #4192, 2.500000000000002220 ) ;
#8356 = DIRECTION ( 'NONE',  ( 0.000000000000000000, 0.000000000000000000, 1.000000000000000000 ) ) ;
#8357 = DIRECTION ( 'NONE',  ( -3.916739600140467622E-15, 1.000000000000000000, 0.000000000000000000 ) ) ;
#8358 =( NAMED_UNIT ( * ) PLANE_ANGLE_UNIT ( ) SI_UNIT ( $, .RADIAN. ) );
#8359 = ORIENTED_EDGE ( 'NONE', *, *, #11603, .T. ) ;
#8360 = PLANE ( 'NONE',  #12784 ) ;
#8361 = CIRCLE ( 'NONE', #10234, 4.000000000000000000 ) ;
#8362 = EDGE_CURVE ( 'NONE', #7974, #4218, #12023, .T. ) ;
#8363 = DIRECTION ( 'NONE',  ( -1.000000000000000000, 0.000000000000000000, 0.000000000000000000 ) ) ;
#8364 = ORIENTED_EDGE ( 'NONE', *, *, #14279, .F. ) ;
#8365 = DIRECTION ( 'NONE',  ( 0.000000000000000000, 0.000000000000000000, -1.000000000000000000 ) ) ;
#8366 = CARTESIAN_POINT ( 'NONE',  ( -118.6817075744281595, 69.57655509336025546, 3.299999999999976730 ) ) ;
#8367 = DIRECTION ( 'NONE',  ( 1.000000000000000000, 0.000000000000000000, 0.000000000000000000 ) ) ;
#8368 = ORIENTED_EDGE ( 'NONE', *, *, #7934, .F. ) ;
#8369 = CARTESIAN_POINT ( 'NONE',  ( 108.6817075744280174, 69.57655509336049704, -3.299999999999981171 ) ) ;
#8370 = AXIS2_PLACEMENT_3D ( 'NONE', #5894, #6732, #12307 ) ;
#8371 = CARTESIAN_POINT ( 'NONE',  ( 4.844561581013658191, 3.861881939214527826, 1.311024268447660290 ) ) ;
#8372 = AXIS2_PLACEMENT_3D ( 'NONE', #1212, #9996, #5591 ) ;
#8373 = CONICAL_SURFACE ( 'NONE', #13971, 5.000000000000000888, 0.9110539511682884672 ) ;
#8374 = DIRECTION ( 'NONE',  ( -2.273843122241288438E-18, -5.551115123125783935E-17, -1.000000000000000000 ) ) ;
#8375 = ORIENTED_EDGE ( 'NONE', *, *, #8242, .F. ) ;
#8376 = ORIENTED_EDGE ( 'NONE', *, *, #12229, .F. ) ;
#8377 = DIRECTION ( 'NONE',  ( 0.000000000000000000, -1.000000000000000000, 0.000000000000000000 ) ) ;
#8378 = CARTESIAN_POINT ( 'NONE',  ( 53.99999999999997868, -1.084202172485504434E-15, -25.00000000000000000 ) ) ;
#8379 = ORIENTED_EDGE ( 'NONE', *, *, #10209, .F. ) ;
#8380 = DIRECTION ( 'NONE',  ( 0.000000000000000000, 0.000000000000000000, 1.000000000000000000 ) ) ;
#8381 = DIRECTION ( 'NONE',  ( 0.9396926207859144231, 2.715694135728174035E-16, -0.3420201433256524481 ) ) ;
#8382 = ADVANCED_FACE ( 'NONE', ( #5663 ), #10142, .F. ) ;
#8383 = DIRECTION ( 'NONE',  ( -0.000000000000000000, 0.000000000000000000, -1.000000000000000000 ) ) ;
#8384 = EDGE_CURVE ( 'NONE', #11506, #25, #261, .T. ) ;
#8385 = CARTESIAN_POINT ( 'NONE',  ( -108.6817075744280316, -30.42344490663957401, -32.00000000000002842 ) ) ;
#8386 = CARTESIAN_POINT ( 'NONE',  ( 60.00000000000000000, -6.123233995736768255E-16, -25.00000000000000000 ) ) ;
#8387 = FACE_BOUND ( 'NONE', #919, .T. ) ;
#8388 = CARTESIAN_POINT ( 'NONE',  ( 20.00000000000000711, 20.00000000000000355, 25.00000000000000000 ) ) ;
#8389 = ORIENTED_EDGE ( 'NONE', *, *, #5237, .T. ) ;
#8390 = VERTEX_POINT ( 'NONE', #13883 ) ;
#8391 = AXIS2_PLACEMENT_3D ( 'NONE', #4542, #5605, #11247 ) ;
#8392 = FACE_OUTER_BOUND ( 'NONE', #6105, .T. ) ;
#8393 = VERTEX_POINT ( 'NONE', #4732 ) ;
#8394 = VERTEX_POINT ( 'NONE', #10500 ) ;
#8395 = DIRECTION ( 'NONE',  ( 0.000000000000000000, 0.000000000000000000, 1.000000000000000000 ) ) ;
#8396 = VECTOR ( 'NONE', #14060, 1000.000000000000000 ) ;
#8397 = CARTESIAN_POINT ( 'NONE',  ( -2.000000000000001776, -3.464101615137750390, 0.000000000000000000 ) ) ;
#8398 = CARTESIAN_POINT ( 'NONE',  ( 31.80000000000005045, 6.938893903907228378E-15, 2.775557561562891351E-14 ) ) ;
#8399 = FACE_OUTER_BOUND ( 'NONE', #2835, .T. ) ;
#8400 = CARTESIAN_POINT ( 'NONE',  ( 5.013196232911404593, -2.310564645009324902, -4.002015359328471966 ) ) ;
#8401 = DIRECTION ( 'NONE',  ( 0.000000000000000000, 0.000000000000000000, -1.000000000000000000 ) ) ;
#8402 = DIRECTION ( 'NONE',  ( 0.000000000000000000, 0.000000000000000000, -1.000000000000000000 ) ) ;
#8403 = CARTESIAN_POINT ( 'NONE',  ( -1.752700365193367750E-15, -5.773502691896300831, -6.000000000000005329 ) ) ;
#8404 = B_SPLINE_CURVE_WITH_KNOTS ( 'NONE', 3,
 ( #9840, #4096, #14244, #14389, #3195, #8743 ),
 .UNSPECIFIED., .F., .F.,
 ( 4, 2, 4 ),
 ( 0.002452478801916362430, 0.003676905084147999610, 0.004901331366379636789 ),
 .UNSPECIFIED. ) ;
#8405 = DIRECTION ( 'NONE',  ( 0.000000000000000000, 1.000000000000000000, 0.000000000000000000 ) ) ;
#8406 = VECTOR ( 'NONE', #13626, 1000.000000000000000 ) ;
#8407 = ORIENTED_EDGE ( 'NONE', *, *, #4693, .T. ) ;
#8408 = LINE ( 'NONE', #5119, #6828 ) ;
#8409 = ORIENTED_EDGE ( 'NONE', *, *, #3124, .F. ) ;
#8410 = ORIENTED_EDGE ( 'NONE', *, *, #4773, .F. ) ;
#8411 = EDGE_CURVE ( 'NONE', #13436, #8560, #2043, .T. ) ;
#8412 = AXIS2_PLACEMENT_3D ( 'NONE', #2849, #12952, #9712 ) ;
#8413 = VECTOR ( 'NONE', #13872, 1000.000000000000114 ) ;
#8414 = PLANE ( 'NONE',  #7593 ) ;
#8415 = CARTESIAN_POINT ( 'NONE',  ( 20.00000000000000000, -5.510910596163090344E-15, 25.00000000000000000 ) ) ;
#8416 = ADVANCED_FACE ( 'NONE', ( #404 ), #388, .F. ) ;
#8417 = ADVANCED_FACE ( 'NONE', ( #8004 ), #482, .T. ) ;
#8418 = ORIENTED_EDGE ( 'NONE', *, *, #7459, .T. ) ;
#8419 = ORIENTED_EDGE ( 'NONE', *, *, #3583, .T. ) ;
#8420 = CARTESIAN_POINT ( 'NONE',  ( 4.400655246570930323, -3.515428273946614723, -4.476900509771775560 ) ) ;
#8421 = VECTOR ( 'NONE', #4332, 1000.000000000000114 ) ;
#8422 = COLOUR_RGB ( '', 0.09019608, 0.27058824, 0.51372549) ;
#8423 = CARTESIAN_POINT ( 'NONE',  ( 0.000000000000000000, 0.000000000000000000, 0.000000000000000000 ) ) ;
#8424 = EDGE_LOOP ( 'NONE', ( #344, #10206, #12578, #4371, #146, #9198, #13128, #9967 ) ) ;
#8425 = CARTESIAN_POINT ( 'NONE',  ( 57.35294117647057277, -1.411764705882362358, -25.00000000000000000 ) ) ;
#8426 = AXIS2_PLACEMENT_3D ( 'NONE', #689, #13059, #6514 ) ;
#8427 = EDGE_CURVE ( 'NONE', #9564, #6762, #336, .T. ) ;
#8428 = VECTOR ( 'NONE', #5043, 1000.000000000000000 ) ;
#8429 = CARTESIAN_POINT ( 'NONE',  ( 0.000000000000000000, 0.000000000000000000, 1.599999999999990319 ) ) ;
#8430 = CARTESIAN_POINT ( 'NONE',  ( 0.000000000000000000, 0.000000000000000000, -35.00000000000000000 ) ) ;
#8431 = DIRECTION ( 'NONE',  ( 0.000000000000000000, 0.000000000000000000, -1.000000000000000000 ) ) ;
#8432 = ORIENTED_EDGE ( 'NONE', *, *, #1152, .T. ) ;
#8433 = CIRCLE ( 'NONE', #2141, 0.4999999999999978351 ) ;
#8434 = FACE_OUTER_BOUND ( 'NONE', #13665, .T. ) ;
#8435 = STYLED_ITEM ( 'NONE', ( #2246 ), #11686 ) ;
#8436 = DIRECTION ( 'NONE',  ( 0.2425356250363304988, -0.9701425001453325425, -0.000000000000000000 ) ) ;
#8437 =( NAMED_UNIT ( * ) SI_UNIT ( $, .STERADIAN. ) SOLID_ANGLE_UNIT ( ) );
#8438 = ADVANCED_FACE ( 'NONE', ( #1503 ), #13969, .T. ) ;
#8439 = ORIENTED_EDGE ( 'NONE', *, *, #1500, .T. ) ;
#8440 = CARTESIAN_POINT ( 'NONE',  ( 3.401922400370811506, 3.809401878279405462, -4.271474537231044089 ) ) ;
#8441 = CARTESIAN_POINT ( 'NONE',  ( -88.22284556172397174, 29.57655509336047572, -117.0000000000000000 ) ) ;
#8442 = ORIENTED_EDGE ( 'NONE', *, *, #5682, .T. ) ;
#8443 = DIRECTION ( 'NONE',  ( 1.000000000000000000, 1.224646799147353454E-16, 0.000000000000000000 ) ) ;
#8444 = LINE ( 'NONE', #2907, #13980 ) ;
#8445 = DIRECTION ( 'NONE',  ( 0.2425356250363327471, -0.9701425001453319874, -0.000000000000000000 ) ) ;
#8446 = VERTEX_POINT ( 'NONE', #3703 ) ;
#8447 = PLANE ( 'NONE',  #5318 ) ;
#8448 = AXIS2_PLACEMENT_3D ( 'NONE', #12001, #6352, #10829 ) ;
#8449 = DIRECTION ( 'NONE',  ( 0.2425356250363330801, -0.9701425001453319874, -0.000000000000000000 ) ) ;
#8450 = COLOUR_RGB ( '', 0.08235294, 0.09019608, 0.10196078) ;
#8451 = CARTESIAN_POINT ( 'NONE',  ( 25.00000000000000000, 199.5765550933606107, 47.99999999999998579 ) ) ;
#8452 = ORIENTED_EDGE ( 'NONE', *, *, #8108, .T. ) ;
#8453 = EDGE_CURVE ( 'NONE', #6345, #588, #1423, .T. ) ;
#8454 = EDGE_LOOP ( 'NONE', ( #6608, #1540, #13407, #3149 ) ) ;
#8455 = CARTESIAN_POINT ( 'NONE',  ( 0.000000000000000000, -2.375000000000000000, -4.362804221962446556E-16 ) ) ;
#8456 = CARTESIAN_POINT ( 'NONE',  ( -2.647226096189655209, 48.05180945724376329, 0.9903388192220039521 ) ) ;
#8457 = VERTEX_POINT ( 'NONE', #4938 ) ;
#8458 = CARTESIAN_POINT ( 'NONE',  ( 3.880206590543185285, 3.396506438958528218, -1.117078279489001735 ) ) ;
#8459 = LINE ( 'NONE', #4950, #10207 ) ;
#8460 = CIRCLE ( 'NONE', #10807, 2.500000000000002220 ) ;
#8461 = FACE_OUTER_BOUND ( 'NONE', #4983, .T. ) ;
#8462 = ADVANCED_FACE ( 'NONE', ( #9401 ), #11311, .F. ) ;
#8463 = VECTOR ( 'NONE', #2524, 1000.000000000000000 ) ;
#8464 = CARTESIAN_POINT ( 'NONE',  ( 4.086262418390194995, -2.102635014057366636, 3.499999999999993339 ) ) ;
#8465 = AXIS2_PLACEMENT_3D ( 'NONE', #4813, #425, #9117 ) ;
#8466 = VECTOR ( 'NONE', #8907, 1000.000000000000000 ) ;
#8467 = ORIENTED_EDGE ( 'NONE', *, *, #11383, .F. ) ;
#8468 = DIRECTION ( 'NONE',  ( -0.000000000000000000, -0.000000000000000000, -1.000000000000000000 ) ) ;
#8469 = CARTESIAN_POINT ( 'NONE',  ( 129.3408537872138595, 189.5765550933606107, -9.000000000000007105 ) ) ;
#8470 = CARTESIAN_POINT ( 'NONE',  ( 4.598786737361985288, -3.118391931134659956, -0.4203182062997378177 ) ) ;
#8471 = ORIENTED_EDGE ( 'NONE', *, *, #8121, .F. ) ;
#8472 = MECHANICAL_DESIGN_GEOMETRIC_PRESENTATION_REPRESENTATION (  '', ( #5879 ), #10337 ) ;
#8473 = EDGE_CURVE ( 'NONE', #11431, #12337, #5994, .T. ) ;
#8474 = VECTOR ( 'NONE', #8998, 1000.000000000000000 ) ;
#8475 = ADVANCED_FACE ( 'NONE', ( #1348 ), #5794, .F. ) ;
#8476 = VECTOR ( 'NONE', #13412, 1000.000000000000000 ) ;
#8477 = ORIENTED_EDGE ( 'NONE', *, *, #7153, .T. ) ;
#8478 = DIRECTION ( 'NONE',  ( -0.9240638205168504316, -0.3822382184081047352, 0.000000000000000000 ) ) ;
#8479 = ORIENTED_EDGE ( 'NONE', *, *, #11129, .F. ) ;
#8480 = ORIENTED_EDGE ( 'NONE', *, *, #6356, .F. ) ;
#8481 = FACE_OUTER_BOUND ( 'NONE', #11329, .T. ) ;
#8482 = CARTESIAN_POINT ( 'NONE',  ( 36.99999999999999289, 80.00000000000000000, 25.00000000000000000 ) ) ;
#8483 = CARTESIAN_POINT ( 'NONE',  ( 1.790396195872467677, 48.30096731618027661, 7.586517658982192103 ) ) ;
#8484 = FACE_OUTER_BOUND ( 'NONE', #10475, .T. ) ;
#8485 = LINE ( 'NONE', #1901, #1437 ) ;
#8486 = DIRECTION ( 'NONE',  ( 1.000000000000000000, 0.000000000000000000, 0.000000000000000000 ) ) ;
#8487 = CARTESIAN_POINT ( 'NONE',  ( 0.000000000000000000, 0.000000000000000000, 25.00000000000000000 ) ) ;
#8488 = AXIS2_PLACEMENT_3D ( 'NONE', #13009, #8740, #6455 ) ;
#8489 = ORIENTED_EDGE ( 'NONE', *, *, #12362, .F. ) ;
#8490 = DIRECTION ( 'NONE',  ( 1.000000000000000000, 0.000000000000000000, 0.000000000000000000 ) ) ;
#8491 = EDGE_CURVE ( 'NONE', #7727, #1356, #3539, .T. ) ;
#8492 = ORIENTED_EDGE ( 'NONE', *, *, #12937, .T. ) ;
#8493 =( REPRESENTATION_RELATIONSHIP ('NONE','NONE', #10295, #7389 ) REPRESENTATION_RELATIONSHIP_WITH_TRANSFORMATION ( #1011 )SHAPE_REPRESENTATION_RELATIONSHIP( ) );
#8494 = EDGE_LOOP ( 'NONE', ( #2950, #14007 ) ) ;
#8495 = AXIS2_PLACEMENT_3D ( 'NONE', #3774, #13730, #1346 ) ;
#8496 = CARTESIAN_POINT ( 'NONE',  ( 20.00000000000000000, -5.510910596163090344E-15, 25.00000000000000000 ) ) ;
#8497 = CARTESIAN_POINT ( 'NONE',  ( 0.000000000000000000, 0.000000000000000000, 0.000000000000000000 ) ) ;
#8498 = AXIS2_PLACEMENT_3D ( 'NONE', #4174, #6477, #4112 ) ;
#8499 = ORIENTED_EDGE ( 'NONE', *, *, #9960, .F. ) ;
#8500 = AXIS2_PLACEMENT_3D ( 'NONE', #7827, #7899, #12444 ) ;
#8501 = CARTESIAN_POINT ( 'NONE',  ( 1.582370436564208838, -4.859920694388245366, -4.019399823475544586 ) ) ;
#8502 = CARTESIAN_POINT ( 'NONE',  ( -3.514986608502201904, -4.017641317387708355, -4.357689166958490290 ) ) ;
#8503 = VERTEX_POINT ( 'NONE', #14239 ) ;
#8504 = ORIENTED_EDGE ( 'NONE', *, *, #9227, .T. ) ;
#8505 = CARTESIAN_POINT ( 'NONE',  ( 108.6817075744280743, 59.57655509336061073, -25.00000000000000000 ) ) ;
#8506 = VECTOR ( 'NONE', #11977, 1000.000000000000000 ) ;
#8507 = EDGE_CURVE ( 'NONE', #11163, #11047, #10723, .T. ) ;
#8508 = UNCERTAINTY_MEASURE_WITH_UNIT (LENGTH_MEASURE( 1.000000000000000082E-05 ), #7132, 'distance_accuracy_value', 'NONE');
#8509 = CARTESIAN_POINT ( 'NONE',  ( 4.000000000000003553, -2.309401076758511806, -3.133295621305376422 ) ) ;
#8510 = DIRECTION ( 'NONE',  ( 0.000000000000000000, 0.000000000000000000, -1.000000000000000000 ) ) ;
#8511 = ADVANCED_FACE ( 'NONE', ( #3188 ), #1725, .F. ) ;
#8512 = DIRECTION ( 'NONE',  ( 0.000000000000000000, 0.000000000000000000, -1.000000000000000000 ) ) ;
#8513 = ORIENTED_EDGE ( 'NONE', *, *, #10574, .F. ) ;
#8514 = CARTESIAN_POINT ( 'NONE',  ( -5.238704763094644612, -1.015773027556925223, -4.385839086323478853 ) ) ;
#8515 = CARTESIAN_POINT ( 'NONE',  ( 5.085139694532330168, -2.386562117782604631, -4.000000000000001776 ) ) ;
#8516 = ORIENTED_EDGE ( 'NONE', *, *, #11605, .F. ) ;
#8517 = EDGE_CURVE ( 'NONE', #5669, #14098, #5540, .T. ) ;
#8518 = DIRECTION ( 'NONE',  ( -1.000000000000000000, -1.665334536937734071E-16, 0.000000000000000000 ) ) ;
#8519 = ORIENTED_EDGE ( 'NONE', *, *, #11066, .F. ) ;
#8520 = ORIENTED_EDGE ( 'NONE', *, *, #6756, .T. ) ;
#8521 = CARTESIAN_POINT ( 'NONE',  ( 20.00000000000000000, 5.000000000000000000, -25.00000000000000000 ) ) ;
#8522 = ADVANCED_FACE ( 'NONE', ( #1870 ), #6324, .F. ) ;
#8523 = LINE ( 'NONE', #4299, #8703 ) ;
#8524 = ORIENTED_EDGE ( 'NONE', *, *, #11879, .F. ) ;
#8525 = DIRECTION ( 'NONE',  ( 1.000000000000000000, 0.000000000000000000, 0.000000000000000000 ) ) ;
#8526 = CARTESIAN_POINT ( 'NONE',  ( 4.988724804725896966, -2.309401076758484272, 4.000000000000003553 ) ) ;
#8527 = ORIENTED_EDGE ( 'NONE', *, *, #3243, .F. ) ;
#8528 = EDGE_CURVE ( 'NONE', #4078, #12827, #4840, .T. ) ;
#8529 = ORIENTED_EDGE ( 'NONE', *, *, #1088, .T. ) ;
#8530 = ORIENTED_EDGE ( 'NONE', *, *, #6270, .F. ) ;
#8531 = CARTESIAN_POINT ( 'NONE',  ( 108.6817075744280174, -20.42344490663938572, 33.00000000000002842 ) ) ;
#8532 = DIRECTION ( 'NONE',  ( 0.000000000000000000, 0.000000000000000000, 1.000000000000000000 ) ) ;
#8533 = ORIENTED_EDGE ( 'NONE', *, *, #6620, .F. ) ;
#8534 = CARTESIAN_POINT ( 'NONE',  ( 4.142654963991842187, -4.070796997468695722, -6.939432481254059658E-15 ) ) ;
#8535 = DIRECTION ( 'NONE',  ( 1.000000000000000000, -0.000000000000000000, -0.000000000000000000 ) ) ;
#8536 = CARTESIAN_POINT ( 'NONE',  ( 2.500000000000002220, 7.224953340212723619E-16, -4.674599999999973221 ) ) ;
#8537 = LINE ( 'NONE', #2994, #2776 ) ;
#8538 = ORIENTED_EDGE ( 'NONE', *, *, #9196, .F. ) ;
#8539 = DIRECTION ( 'NONE',  ( 1.000000000000000000, 0.000000000000000000, 0.000000000000000000 ) ) ;
#8540 = CARTESIAN_POINT ( 'NONE',  ( 54.35294117647056567, -1.411764705882362358, 23.00000000000000000 ) ) ;
#8541 = ADVANCED_FACE ( 'NONE', ( #9700 ), #9753, .T. ) ;
#8542 = CARTESIAN_POINT ( 'NONE',  ( 0.000000000000000000, 40.49999999999999289, 0.000000000000000000 ) ) ;
#8543 = ORIENTED_EDGE ( 'NONE', *, *, #12426, .F. ) ;
#8544 = EDGE_CURVE ( 'NONE', #9291, #1178, #5079, .T. ) ;
#8545 = VERTEX_POINT ( 'NONE', #11751 ) ;
#8546 = CARTESIAN_POINT ( 'NONE',  ( 5.099999999999993427, 0.000000000000000000, 0.000000000000000000 ) ) ;
#8547 = EDGE_LOOP ( 'NONE', ( #1850, #5601, #1892, #5905 ) ) ;
#8548 = ORIENTED_EDGE ( 'NONE', *, *, #3432, .F. ) ;
#8549 = CARTESIAN_POINT ( 'NONE',  ( -31.96535124910143821, 127.8614049964057813, 1.219362754841566419E-12 ) ) ;
#8550 = DIRECTION ( 'NONE',  ( -0.2425356250363330801, 0.9701425001453319874, 0.000000000000000000 ) ) ;
#8551 = CARTESIAN_POINT ( 'NONE',  ( 0.000000000000000000, 48.49999999999999289, 8.000000000000007105 ) ) ;
#8552 = AXIS2_PLACEMENT_3D ( 'NONE', #9001, #6665, #5567 ) ;
#8553 = CARTESIAN_POINT ( 'NONE',  ( 5.091953023115924459, -2.341213539480245576, -4.055100801747961725 ) ) ;
#8554 = DIRECTION ( 'NONE',  ( 0.000000000000000000, 0.000000000000000000, 1.000000000000000000 ) ) ;
#8555 = APPLICATION_PROTOCOL_DEFINITION ( 'draft international standard', 'automotive_design', 1998, #645 ) ;
#8556 = CARTESIAN_POINT ( 'NONE',  ( -88.22284556172397174, 29.57655509336047572, 33.00000000000002842 ) ) ;
#8557 = EDGE_CURVE ( 'NONE', #11484, #5967, #1646, .T. ) ;
#8558 = DIRECTION ( 'NONE',  ( 0.000000000000000000, 0.000000000000000000, -1.000000000000000000 ) ) ;
#8559 = CARTESIAN_POINT ( 'NONE',  ( -5.551115123125782702E-14, -3.464101615137743728, -2.000000000000015543 ) ) ;
#8560 = VERTEX_POINT ( 'NONE', #8369 ) ;
#8561 = EDGE_LOOP ( 'NONE', ( #13814, #13690, #8885, #10525 ) ) ;
#8562 = VERTEX_POINT ( 'NONE', #13076 ) ;
#8563 = VECTOR ( 'NONE', #8713, 1000.000000000000000 ) ;
#8564 = LINE ( 'NONE', #4054, #775 ) ;
#8565 = CARTESIAN_POINT ( 'NONE',  ( 0.000000000000000000, 1.387778780781445676E-14, 3.499999999999982236 ) ) ;
#8566 = EDGE_CURVE ( 'NONE', #11544, #6869, #1729, .T. ) ;
#8567 = EDGE_CURVE ( 'NONE', #1326, #1181, #10863, .T. ) ;
#8568 = CARTESIAN_POINT ( 'NONE',  ( 3.417629563435787610, -3.800333343456214319, -4.019399823475544586 ) ) ;
#8569 = DIRECTION ( 'NONE',  ( 0.000000000000000000, 0.000000000000000000, 1.000000000000000000 ) ) ;
#8570 = CARTESIAN_POINT ( 'NONE',  ( 68.68170757442801744, -83.66032599071898801, 33.00000000000002842 ) ) ;
#8571 = EDGE_CURVE ( 'NONE', #4249, #14186, #6710, .T. ) ;
#8572 = ORIENTED_EDGE ( 'NONE', *, *, #11196, .T. ) ;
#8573 = FACE_OUTER_BOUND ( 'NONE', #6953, .T. ) ;
#8574 = CARTESIAN_POINT ( 'NONE',  ( 5.244800587397359770, 2.026986389275614364, -4.490560292650632945 ) ) ;
#8575 = DIRECTION ( 'NONE',  ( -1.000000000000000000, 0.000000000000000000, 0.000000000000000000 ) ) ;
#8576 = ORIENTED_EDGE ( 'NONE', *, *, #2998, .F. ) ;
#8577 = DIRECTION ( 'NONE',  ( 0.000000000000000000, 0.000000000000000000, -1.000000000000000000 ) ) ;
#8578 = CARTESIAN_POINT ( 'NONE',  ( 5.108576695057072570, 2.381536396098283159, -4.077513086864523295 ) ) ;
#8579 = EDGE_LOOP ( 'NONE', ( #4612, #13877, #3353, #9448, #5302 ) ) ;
#8580 = CARTESIAN_POINT ( 'NONE',  ( 0.000000000000000000, 189.5765550933606107, -32.00000000000002842 ) ) ;
#8581 = VECTOR ( 'NONE', #3337, 1000.000000000000114 ) ;
#8582 = EDGE_LOOP ( 'NONE', ( #12881, #6061, #8912, #13388 ) ) ;
#8583 = ADVANCED_FACE ( 'NONE', ( #7477 ), #11624, .T. ) ;
#8584 = VERTEX_POINT ( 'NONE', #638 ) ;
#8585 = CARTESIAN_POINT ( 'NONE',  ( 25.90000000000000213, 29.99999999999999645, 6.999999999999992006 ) ) ;
#8586 = CARTESIAN_POINT ( 'NONE',  ( 53.99999999999997868, -1.347111479062091166E-15, 25.00000000000000000 ) ) ;
#8587 = ORIENTED_EDGE ( 'NONE', *, *, #898, .F. ) ;
#8588 = DIRECTION ( 'NONE',  ( 0.000000000000000000, 0.4999999999999996669, 0.8660254037844388186 ) ) ;
#8589 = CARTESIAN_POINT ( 'NONE',  ( 5.000000000000005329, -2.886751345948144643, -4.369522543421425098 ) ) ;
#8590 = VECTOR ( 'NONE', #2350, 1000.000000000000000 ) ;
#8591 = ORIENTED_EDGE ( 'NONE', *, *, #150, .T. ) ;
#8592 = AXIS2_PLACEMENT_3D ( 'NONE', #1295, #5738, #11390 ) ;
#8593 = EDGE_LOOP ( 'NONE', ( #12591, #5897, #12415, #6047, #6425, #12852, #5145, #6101, #1637, #5793 ) ) ;
#8594 = CARTESIAN_POINT ( 'NONE',  ( -0.6920835326022490852, -4.454600218803899558, -3.297382984111598692 ) ) ;
#8595 = CARTESIAN_POINT ( 'NONE',  ( -3.464648251117637301, 47.71258338693829160, 1.984273587230471314 ) ) ;
#8596 = EDGE_LOOP ( 'NONE', ( #8127, #12236, #7359, #8634 ) ) ;
#8597 = CARTESIAN_POINT ( 'NONE',  ( 4.132952817037849336, -4.063368025374519910, -6.938893903907228378E-15 ) ) ;
#8598 = PRODUCT_DEFINITION_SHAPE ( 'NONE', 'NONE',  #14479 ) ;
#8599 = CARTESIAN_POINT ( 'NONE',  ( 0.000000000000000000, 25.49999999999996803, 8.000000000000007105 ) ) ;
#8600 = CARTESIAN_POINT ( 'NONE',  ( 4.180345472528537165, 2.086001522971432820, 3.570468649087204849 ) ) ;
#8601 = EDGE_LOOP ( 'NONE', ( #10801, #13101, #1734, #5899 ) ) ;
#8602 = FACE_OUTER_BOUND ( 'NONE', #3044, .T. ) ;
#8603 = EDGE_CURVE ( 'NONE', #4249, #11970, #4401, .T. ) ;
#8604 = ADVANCED_FACE ( 'NONE', ( #2912 ), #9556, .T. ) ;
#8605 = CIRCLE ( 'NONE', #2298, 2.500000000000002220 ) ;
#8606 = CARTESIAN_POINT ( 'NONE',  ( 40.00000000000000711, 80.00000000000000000, 25.00000000000000000 ) ) ;
#8607 = VECTOR ( 'NONE', #12624, 1000.000000000000000 ) ;
#8608 = CARTESIAN_POINT ( 'NONE',  ( 4.630153689607063860, -2.981509523526843174E-16, -5.371010071662830399 ) ) ;
#8609 = VECTOR ( 'NONE', #43, 1000.000000000000000 ) ;
#8610 = ADVANCED_FACE ( 'NONE', ( #4000 ), #8447, .F. ) ;
#8611 = ORIENTED_EDGE ( 'NONE', *, *, #8310, .F. ) ;
#8612 = ORIENTED_EDGE ( 'NONE', *, *, #6831, .T. ) ;
#8613 = EDGE_LOOP ( 'NONE', ( #9864, #2166 ) ) ;
#8614 = DIRECTION ( 'NONE',  ( -0.2425356250363330801, 0.9701425001453319874, 0.000000000000000000 ) ) ;
#8615 = ORIENTED_EDGE ( 'NONE', *, *, #8273, .F. ) ;
#8616 = EDGE_CURVE ( 'NONE', #5269, #14306, #9622, .T. ) ;
#8617 = EDGE_CURVE ( 'NONE', #14306, #6762, #7618, .T. ) ;
#8618 = VERTEX_POINT ( 'NONE', #1056 ) ;
#8619 = AXIS2_PLACEMENT_3D ( 'NONE', #3718, #2613, #7362 ) ;
#8620 = CARTESIAN_POINT ( 'NONE',  ( 27.30499999999998195, 0.000000000000000000, 2.499999999999999556 ) ) ;
#8621 = DIRECTION ( 'NONE',  ( 0.000000000000000000, 0.000000000000000000, 1.000000000000000000 ) ) ;
#8622 = ORIENTED_EDGE ( 'NONE', *, *, #4123, .T. ) ;
#8623 = CARTESIAN_POINT ( 'NONE',  ( 3.587774770580208106, 47.65128983029576659, 2.212041269487582618 ) ) ;
#8624 = CARTESIAN_POINT ( 'NONE',  ( 5.733169058567799681, -6.938893903907228378E-15, 0.000000000000000000 ) ) ;
#8625 = CARTESIAN_POINT ( 'NONE',  ( 108.6817075744280174, -20.42344490663938572, 33.00000000000002842 ) ) ;
#8626 = APPLICATION_PROTOCOL_DEFINITION ( 'draft international standard', 'automotive_design', 1998, #12124 ) ;
#8627 = CARTESIAN_POINT ( 'NONE',  ( 4.211399264691415567, -2.459727859270663952, -3.451161839612804094 ) ) ;
#8628 = CARTESIAN_POINT ( 'NONE',  ( 54.35294117647056567, -1.411764705882362358, 25.00000000000000000 ) ) ;
#8629 = ORIENTED_EDGE ( 'NONE', *, *, #3809, .F. ) ;
#8630 = CARTESIAN_POINT ( 'NONE',  ( 0.000000000000000000, 25.49999999999996803, 0.000000000000000000 ) ) ;
#8631 = VECTOR ( 'NONE', #12385, 1000.000000000000000 ) ;
#8632 = ORIENTED_EDGE ( 'NONE', *, *, #11989, .F. ) ;
#8633 = VECTOR ( 'NONE', #12966, 1000.000000000000000 ) ;
#8634 = ORIENTED_EDGE ( 'NONE', *, *, #9945, .F. ) ;
#8635 = EDGE_CURVE ( 'NONE', #10731, #3393, #14310, .T. ) ;
#8636 = ORIENTED_EDGE ( 'NONE', *, *, #9210, .T. ) ;
#8637 = DIRECTION ( 'NONE',  ( -1.000000000000000000, 2.551526159633733968E-19, 1.987661601597216239E-18 ) ) ;
#8638 = DIRECTION ( 'NONE',  ( -0.9701425001453318764, -0.2425356250363329969, 0.000000000000000000 ) ) ;
#8639 = FACE_OUTER_BOUND ( 'NONE', #5745, .T. ) ;
#8640 = AXIS2_PLACEMENT_3D ( 'NONE', #13177, #10886, #14059 ) ;
#8641 = ORIENTED_EDGE ( 'NONE', *, *, #13064, .F. ) ;
#8642 = PLANE ( 'NONE',  #1349 ) ;
#8643 = CARTESIAN_POINT ( 'NONE',  ( 4.451998719175967729E-15, 5.807445019730661961, -4.451004066889661104 ) ) ;
#8644 = CARTESIAN_POINT ( 'NONE',  ( 18.68170757442808849, 141.2731697022877313, -35.00000000000000000 ) ) ;
#8645 = CIRCLE ( 'NONE', #4475, 2.500000000000002220 ) ;
#8646 = EDGE_CURVE ( 'NONE', #1328, #8838, #11612, .T. ) ;
#8647 = UNCERTAINTY_MEASURE_WITH_UNIT (LENGTH_MEASURE( 1.000000000000000082E-05 ), #6065, 'distance_accuracy_value', 'NONE');
#8648 = PRODUCT_RELATED_PRODUCT_CATEGORY ( 'part', '', ( #10212 ) ) ;
#8649 = EDGE_CURVE ( 'NONE', #10570, #10136, #3002, .T. ) ;
#8650 = LINE ( 'NONE', #10913, #9361 ) ;
#8651 = DIRECTION ( 'NONE',  ( -0.000000000000000000, 1.000000000000000000, -0.000000000000000000 ) ) ;
#8652 = CARTESIAN_POINT ( 'NONE',  ( 20.00000000000000355, 17.00000000000000000, 25.00000000000000000 ) ) ;
#8653 = CARTESIAN_POINT ( 'NONE',  ( 20.00000000000000000, -5.510910596163090344E-15, 25.00000000000000000 ) ) ;
#8654 = CARTESIAN_POINT ( 'NONE',  ( 1.999999999999996225, 3.464101615137748613, -2.842992957459213432 ) ) ;
#8655 =( NAMED_UNIT ( * ) SI_UNIT ( $, .STERADIAN. ) SOLID_ANGLE_UNIT ( ) );
#8656 = FACE_BOUND ( 'NONE', #3425, .T. ) ;
#8657 = ORIENTED_EDGE ( 'NONE', *, *, #11542, .T. ) ;
#8658 = PRESENTATION_LAYER_ASSIGNMENT (  '', '', ( #13344 ) ) ;
#8659 = ORIENTED_EDGE ( 'NONE', *, *, #3172, .T. ) ;
#8660 = DIRECTION ( 'NONE',  ( 0.000000000000000000, 1.000000000000000000, 0.000000000000000000 ) ) ;
#8661 = TOROIDAL_SURFACE ( 'NONE', #10537, 3.199999999999998845, 0.8000000000000001554 ) ;
#8662 = DIRECTION ( 'NONE',  ( -1.000000000000000000, 0.000000000000000000, 0.000000000000000000 ) ) ;
#8663 = ORIENTED_EDGE ( 'NONE', *, *, #8384, .F. ) ;
#8664 = CARTESIAN_POINT ( 'NONE',  ( -3.081487911019577365E-30, 3.469446951953614189E-15, -5.432899837730820636 ) ) ;
#8665 = FACE_BOUND ( 'NONE', #3830, .T. ) ;
#8666 = ORIENTED_EDGE ( 'NONE', *, *, #796, .T. ) ;
#8667 = VECTOR ( 'NONE', #10901, 1000.000000000000000 ) ;
#8668 = AXIS2_PLACEMENT_3D ( 'NONE', #11516, #13666, #5940 ) ;
#8669 = EDGE_LOOP ( 'NONE', ( #7789, #4229, #5992, #5998 ) ) ;
#8670 = CARTESIAN_POINT ( 'NONE',  ( -2.500000000000011990, 4.330127018922186544, 0.000000000000000000 ) ) ;
#8671 = CARTESIAN_POINT ( 'NONE',  ( -1.786241414228626923, 48.30187417244851389, 0.4115279878254325396 ) ) ;
#8672 = ORIENTED_EDGE ( 'NONE', *, *, #9151, .T. ) ;
#8673 = CARTESIAN_POINT ( 'NONE',  ( 4.114405500665252013, -4.051151509359440794, -1.059651684330564515E-16 ) ) ;
#8674 = CARTESIAN_POINT ( 'NONE',  ( -3.081487911019577365E-30, 3.469446951953614189E-15, -5.974599999999997024 ) ) ;
#8675 = LINE ( 'NONE', #12052, #10477 ) ;
#8676 = CARTESIAN_POINT ( 'NONE',  ( 3.878089031707513623, 0.7015470581927707450, 3.499999999999992895 ) ) ;
#8677 = ORIENTED_EDGE ( 'NONE', *, *, #580, .T. ) ;
#8678 = CARTESIAN_POINT ( 'NONE',  ( 0.000000000000000000, 0.000000000000000000, 0.000000000000000000 ) ) ;
#8679 = FACE_OUTER_BOUND ( 'NONE', #5163, .T. ) ;
#8680 = AXIS2_PLACEMENT_3D ( 'NONE', #1306, #5755, #11406 ) ;
#8681 =( GEOMETRIC_REPRESENTATION_CONTEXT ( 3 ) GLOBAL_UNCERTAINTY_ASSIGNED_CONTEXT ( ( #7463 ) ) GLOBAL_UNIT_ASSIGNED_CONTEXT ( ( #12019, #4201, #949 ) ) REPRESENTATION_CONTEXT ( 'NONE', 'WORKASPACE' ) );
#8682 = CIRCLE ( 'NONE', #10308, 4.999999999999976907 ) ;
#8683 = DIRECTION ( 'NONE',  ( 0.000000000000000000, 0.000000000000000000, -1.000000000000000000 ) ) ;
#8684 = ORIENTED_EDGE ( 'NONE', *, *, #8123, .F. ) ;
#8685 = ORIENTED_EDGE ( 'NONE', *, *, #5466, .T. ) ;
#8686 = EDGE_LOOP ( 'NONE', ( #5124, #2676, #5789, #6851 ) ) ;
#8687 = ADVANCED_FACE ( 'NONE', ( #3127 ), #975, .F. ) ;
#8688 = CARTESIAN_POINT ( 'NONE',  ( 4.185558440016316162, 3.356969399843931612, -0.2680587191991122276 ) ) ;
#8689 = ORIENTED_EDGE ( 'NONE', *, *, #11936, .F. ) ;
#8690 = LINE ( 'NONE', #1896, #6993 ) ;
#8691 = AXIS2_PLACEMENT_3D ( 'NONE', #1324, #236, #9306 ) ;
#8692 = AXIS2_PLACEMENT_3D ( 'NONE', #11558, #11287, #13496 ) ;
#8693 = CARTESIAN_POINT ( 'NONE',  ( 22.00000000000000000, 60.00000000000000711, -25.00000000000000000 ) ) ;
#8694 = CARTESIAN_POINT ( 'NONE',  ( 3.789464654225618734, 47.54647181849109927, 5.306690203119769578 ) ) ;
#8695 = DIRECTION ( 'NONE',  ( 0.000000000000000000, 0.5000000000000011102, -0.8660254037844379305 ) ) ;
#8696 = CARTESIAN_POINT ( 'NONE',  ( 28.00000000000000355, 29.99999999999999645, -6.999999999999992006 ) ) ;
#8697 = APPLICATION_PROTOCOL_DEFINITION ( 'draft international standard', 'automotive_design', 1998, #9795 ) ;
#8698 = LINE ( 'NONE', #14413, #5854 ) ;
#8699 = DIRECTION ( 'NONE',  ( 0.000000000000000000, 0.000000000000000000, 1.000000000000000000 ) ) ;
#8700 = EDGE_LOOP ( 'NONE', ( #8389, #2439, #14333, #8442, #5140 ) ) ;
#8701 = AXIS2_PLACEMENT_3D ( 'NONE', #4585, #9016, #5519 ) ;
#8702 = EDGE_CURVE ( 'NONE', #1767, #4731, #2160, .T. ) ;
#8703 = VECTOR ( 'NONE', #8662, 1000.000000000000000 ) ;
#8704 = VECTOR ( 'NONE', #6810, 1000.000000000000000 ) ;
#8705 = CARTESIAN_POINT ( 'NONE',  ( 4.175572532730949860, -2.061029303918042288, 3.569807470274396266 ) ) ;
#8706 = VERTEX_POINT ( 'NONE', #4367 ) ;
#8707 = EDGE_CURVE ( 'NONE', #11445, #6869, #13285, .T. ) ;
#8708 = VERTEX_POINT ( 'NONE', #6453 ) ;
#8709 = ORIENTED_EDGE ( 'NONE', *, *, #7070, .F. ) ;
#8710 = CARTESIAN_POINT ( 'NONE',  ( 0.000000000000000000, 0.000000000000000000, 0.000000000000000000 ) ) ;
#8711 = CARTESIAN_POINT ( 'NONE',  ( -13.00000000000000533, 35.49999999999997158, 8.000000000000007105 ) ) ;
#8712 = CARTESIAN_POINT ( 'NONE',  ( 0.1586754815284918407, 4.240386000424043011, 0.6554360035617904368 ) ) ;
#8713 = DIRECTION ( 'NONE',  ( 0.000000000000000000, 0.000000000000000000, -1.000000000000000000 ) ) ;
#8714 = ORIENTED_EDGE ( 'NONE', *, *, #1819, .F. ) ;
#8715 = LINE ( 'NONE', #13052, #5096 ) ;
#8716 = EDGE_CURVE ( 'NONE', #7073, #32, #3367, .T. ) ;
#8717 = DIRECTION ( 'NONE',  ( 0.000000000000000000, -1.000000000000000000, 0.000000000000000000 ) ) ;
#8718 = LINE ( 'NONE', #8570, #7068 ) ;
#8719 = VECTOR ( 'NONE', #14224, 1000.000000000000000 ) ;
#8720 = PRODUCT_DEFINITION_SHAPE ( 'NONE', 'NONE',  #14481 ) ;
#8721 = CARTESIAN_POINT ( 'NONE',  ( 0.02511946470933534847, -4.877415451931371493, -3.451298686683617500 ) ) ;
#8722 = EDGE_CURVE ( 'NONE', #12012, #12392, #5513, .T. ) ;
#8723 = DIRECTION ( 'NONE',  ( 1.000000000000000000, 0.000000000000000000, 0.000000000000000000 ) ) ;
#8724 = DIRECTION ( 'NONE',  ( -1.000000000000000000, -4.406877377903812337E-17, 0.000000000000000000 ) ) ;
#8725 = DIRECTION ( 'NONE',  ( -1.734723475976770694E-18, 4.440892098500620738E-16, 1.000000000000000000 ) ) ;
#8726 = DIRECTION ( 'NONE',  ( -1.000000000000000000, 0.000000000000000000, 0.000000000000000000 ) ) ;
#8727 = CARTESIAN_POINT ( 'NONE',  ( 5.005339567054419625, -2.401213891501550624, -4.000000000000001776 ) ) ;
#8728 = FACE_OUTER_BOUND ( 'NONE', #9677, .T. ) ;
#8729 = ORIENTED_EDGE ( 'NONE', *, *, #3562, .T. ) ;
#8730 = B_SPLINE_CURVE_WITH_KNOTS ( 'NONE', 3,
 ( #6013, #9024, #2384, #9247, #9320, #11370 ),
 .UNSPECIFIED., .F., .F.,
 ( 4, 2, 4 ),
 ( 0.003358874760055534110, 0.004541967308452078168, 0.005725059856848621793 ),
 .UNSPECIFIED. ) ;
#8731 = ORIENTED_EDGE ( 'NONE', *, *, #13325, .T. ) ;
#8732 = PLANE ( 'NONE',  #10220 ) ;
#8733 = ADVANCED_FACE ( 'NONE', ( #5370 ), #9980, .F. ) ;
#8734 = EDGE_CURVE ( 'NONE', #11470, #36, #8812, .T. ) ;
#8735 = B_SPLINE_CURVE_WITH_KNOTS ( 'NONE', 3,
 ( #9381, #240, #12669, #3905, #1625, #4710 ),
 .UNSPECIFIED., .F., .F.,
 ( 4, 2, 4 ),
 ( -3.988673288085428471E-06, 0.0002483701411510698723, 0.0005007289555902250935 ),
 .UNSPECIFIED. ) ;
#8736 = CARTESIAN_POINT ( 'NONE',  ( 4.141042022537586575, -2.227970427079388305, -3.387027626239151878 ) ) ;
#8737 = VECTOR ( 'NONE', #2236, 1000.000000000000000 ) ;
#8738 = VERTEX_POINT ( 'NONE', #13688 ) ;
#8739 = DIRECTION ( 'NONE',  ( 0.000000000000000000, 0.000000000000000000, -1.000000000000000000 ) ) ;
#8740 = DIRECTION ( 'NONE',  ( 0.000000000000000000, 0.000000000000000000, 1.000000000000000000 ) ) ;
#8741 = ORIENTED_EDGE ( 'NONE', *, *, #3599, .F. ) ;
#8742 = ORIENTED_EDGE ( 'NONE', *, *, #11415, .F. ) ;
#8743 = CARTESIAN_POINT ( 'NONE',  ( 4.211140560182194292, -2.431303136016548017, -3.445885042887453231 ) ) ;
#8744 = DIRECTION ( 'NONE',  ( 0.000000000000000000, 0.000000000000000000, -1.000000000000000000 ) ) ;
#8745 = DIRECTION ( 'NONE',  ( 0.000000000000000000, 8.482162385747133845E-47, -1.000000000000000000 ) ) ;
#8746 = DIRECTION ( 'NONE',  ( -1.000000000000000000, 2.551526159633733968E-19, 1.987661601597216239E-18 ) ) ;
#8747 = LINE ( 'NONE', #988, #12357 ) ;
#8748 = FACE_OUTER_BOUND ( 'NONE', #8295, .T. ) ;
#8749 = VERTEX_POINT ( 'NONE', #3723 ) ;
#8750 = FILL_AREA_STYLE_COLOUR ( '', #2352 ) ;
#8751 = FACE_OUTER_BOUND ( 'NONE', #4316, .T. ) ;
#8752 = EDGE_CURVE ( 'NONE', #3420, #4122, #3653, .T. ) ;
#8753 = EDGE_CURVE ( 'NONE', #2228, #5057, #8165, .T. ) ;
#8754 = CARTESIAN_POINT ( 'NONE',  ( 1.560000000000005826, -0.8660254037844428154, 1.500000000000001332 ) ) ;
#8755 = VERTEX_POINT ( 'NONE', #8086 ) ;
#8756 = EDGE_CURVE ( 'NONE', #981, #1738, #3229, .T. ) ;
#8757 = VERTEX_POINT ( 'NONE', #2549 ) ;
#8758 = CARTESIAN_POINT ( 'NONE',  ( -129.3408537872145132, 189.5765550933606107, -80.00000000000001421 ) ) ;
#8759 = EDGE_LOOP ( 'NONE', ( #8529, #10054 ) ) ;
#8760 = CARTESIAN_POINT ( 'NONE',  ( 4.180345136606687717, -2.085999704580147718, -3.570468642550108207 ) ) ;
#8761 = DIRECTION ( 'NONE',  ( -1.000000000000000000, 0.000000000000000000, 0.000000000000000000 ) ) ;
#8762 = CARTESIAN_POINT ( 'NONE',  ( 2.448955312130046913, 48.11928591936100474, 0.8265499080465862347 ) ) ;
#8763 = PLANE ( 'NONE',  #8111 ) ;
#8764 = FACE_OUTER_BOUND ( 'NONE', #6412, .T. ) ;
#8765 = LINE ( 'NONE', #10962, #7745 ) ;
#8766 =( REPRESENTATION_RELATIONSHIP ('NONE','NONE', #10295, #4344 ) REPRESENTATION_RELATIONSHIP_WITH_TRANSFORMATION ( #4995 )SHAPE_REPRESENTATION_RELATIONSHIP( ) );
#8767 = CARTESIAN_POINT ( 'NONE',  ( 5.103531824934171013, -4.708196996972898063, 1.387778780781445676E-14 ) ) ;
#8768 = EDGE_CURVE ( 'NONE', #6636, #269, #8939, .T. ) ;
#8769 = EDGE_CURVE ( 'NONE', #13012, #3061, #3033, .T. ) ;
#8770 = ORIENTED_EDGE ( 'NONE', *, *, #206, .T. ) ;
#8771 = DIRECTION ( 'NONE',  ( 0.000000000000000000, -0.5000000000000011102, 0.8660254037844380415 ) ) ;
#8772 = VERTEX_POINT ( 'NONE', #9115 ) ;
#8773 = CARTESIAN_POINT ( 'NONE',  ( 20.00000000000000355, 40.00000000000000711, -25.00000000000000000 ) ) ;
#8774 = VECTOR ( 'NONE', #762, 1000.000000000000000 ) ;
#8775 = ORIENTED_EDGE ( 'NONE', *, *, #2503, .F. ) ;
#8776 = CARTESIAN_POINT ( 'NONE',  ( -5.000000000000000000, 0.2466074518009251093, 6.437450399132684549E-16 ) ) ;
#8777 = LINE ( 'NONE', #874, #7692 ) ;
#8778 = ADVANCED_FACE ( 'NONE', ( #6991 ), #8325, .F. ) ;
#8779 = CARTESIAN_POINT ( 'NONE',  ( 0.3572655899082288755, 4.618802153517023612, 1.387778780781445676E-14 ) ) ;
#8780 = DIRECTION ( 'NONE',  ( 1.000000000000000000, -2.551526159633733968E-19, -1.987661601597216239E-18 ) ) ;
#8781 = PLANE ( 'NONE',  #6110 ) ;
#8782 = SURFACE_SIDE_STYLE ('',( #475 ) ) ;
#8783 = EDGE_LOOP ( 'NONE', ( #10305, #6672, #12083, #4013, #12857 ) ) ;
#8784 = EDGE_CURVE ( 'NONE', #7655, #13637, #9984, .T. ) ;
#8785 = EDGE_CURVE ( 'NONE', #7559, #12838, #3015, .T. ) ;
#8786 = DIRECTION ( 'NONE',  ( 0.000000000000000000, 0.000000000000000000, -1.000000000000000000 ) ) ;
#8787 = CARTESIAN_POINT ( 'NONE',  ( 2.749999999999998224, 0.000000000000000000, 2.699999999999999289 ) ) ;
#8788 = CARTESIAN_POINT ( 'NONE',  ( 78.52142056027061301, -86.08568224108226730, 33.00000000000000000 ) ) ;
#8789 = PLANE ( 'NONE',  #13820 ) ;
#8790 = CARTESIAN_POINT ( 'NONE',  ( 4.851472949720940342, -2.694301256218261109, -3.333333333333325932 ) ) ;
#8791 = CARTESIAN_POINT ( 'NONE',  ( 4.767554269344977058, -3.063547535897971574, 2.693780016422239854 ) ) ;
#8792 = CARTESIAN_POINT ( 'NONE',  ( 30.07694101601105530, 130.0000000000000000, 25.00000000000000000 ) ) ;
#8793 = EDGE_CURVE ( 'NONE', #6994, #8314, #14196, .T. ) ;
#8794 = CARTESIAN_POINT ( 'NONE',  ( 76.68170757442801744, 29.57655509336063204, -33.00000000000000000 ) ) ;
#8795 = CARTESIAN_POINT ( 'NONE',  ( 0.000000000000000000, 189.5765550933606107, 0.000000000000000000 ) ) ;
#8796 = B_SPLINE_CURVE_WITH_KNOTS ( 'NONE', 3,
 ( #3407, #11138, #10043, #6600, #13357, #3470, #13435, #14446, #12649, #2290, #2639, #12251, #11209, #12388, #2363, #4897 ),
 .UNSPECIFIED., .F., .F.,
 ( 4, 3, 3, 3, 3, 4 ),
 ( 0.000000000000000000, 3.647308126642597652E-05, 7.269606878412227468E-05, 0.0001129253843484859200, 0.0001515766232005100775, 0.0001537911822990420917 ),
 .UNSPECIFIED. ) ;
#8797 = LINE ( 'NONE', #13279, #3570 ) ;
#8798 = EDGE_LOOP ( 'NONE', ( #683, #4156, #4389, #12824 ) ) ;
#8799 = CIRCLE ( 'NONE', #4386, 2.500000000000002220 ) ;
#8800 = EDGE_LOOP ( 'NONE', ( #13504, #4683, #10409, #7401 ) ) ;
#8801 = FACE_OUTER_BOUND ( 'NONE', #3073, .T. ) ;
#8802 = SHAPE_REPRESENTATION ( 'hex flange bolt small_iso_ISO 4162 - M6 x 25 x 25-C', ( #11025 ), #1942 ) ;
#8803 = SURFACE_SIDE_STYLE ('',( #8945 ) ) ;
#8804 = ORIENTED_EDGE ( 'NONE', *, *, #4368, .T. ) ;
#8805 = CARTESIAN_POINT ( 'NONE',  ( -2.499999999999999556, 4.330127018922202531, -3.920524600599842202 ) ) ;
#8806 = DIRECTION ( 'NONE',  ( 0.000000000000000000, 0.000000000000000000, 1.000000000000000000 ) ) ;
#8807 = ORIENTED_EDGE ( 'NONE', *, *, #4991, .F. ) ;
#8808 = ORIENTED_EDGE ( 'NONE', *, *, #1889, .F. ) ;
#8809 = LINE ( 'NONE', #7485, #1740 ) ;
#8810 = DIRECTION ( 'NONE',  ( 0.000000000000000000, 0.000000000000000000, -1.000000000000000000 ) ) ;
#8811 = EDGE_CURVE ( 'NONE', #588, #375, #14447, .T. ) ;
#8812 = CIRCLE ( 'NONE', #2500, 9.999999999999996447 ) ;
#8813 = CARTESIAN_POINT ( 'NONE',  ( 4.158921614371309694, -4.076055977742311320, 0.05993604794450246853 ) ) ;
#8814 = CARTESIAN_POINT ( 'NONE',  ( -2.344047193898588510, -3.265465875126481787, -1.015423097168454931E-14 ) ) ;
#8815 = LINE ( 'NONE', #4163, #8835 ) ;
#8816 = CARTESIAN_POINT ( 'NONE',  ( 49.47979101891770171, 52.38859998837343568, 25.00000000000000000 ) ) ;
#8817 = DIRECTION ( 'NONE',  ( 0.000000000000000000, -8.482162385747133845E-47, 1.000000000000000000 ) ) ;
#8818 = CARTESIAN_POINT ( 'NONE',  ( -2.931639317407896073, 4.080919942823921787, -0.01465562841807914810 ) ) ;
#8819 = PLANE ( 'NONE',  #12818 ) ;
#8820 = VECTOR ( 'NONE', #2522, 1000.000000000000000 ) ;
#8821 = AXIS2_PLACEMENT_3D ( 'NONE', #8469, #5177, #5251 ) ;
#8822 = VERTEX_POINT ( 'NONE', #1365 ) ;
#8823 = ORIENTED_EDGE ( 'NONE', *, *, #3685, .T. ) ;
#8824 = DIRECTION ( 'NONE',  ( 0.000000000000000000, -4.440892098500619752E-16, -1.000000000000000000 ) ) ;
#8825 = ADVANCED_FACE ( 'NONE', ( #281 ), #353, .F. ) ;
#8826 = ORIENTED_EDGE ( 'NONE', *, *, #14279, .T. ) ;
#8827 = CARTESIAN_POINT ( 'NONE',  ( 4.086375874528097363, -2.103253014742902938, -3.499999999999992895 ) ) ;
#8828 = EDGE_CURVE ( 'NONE', #13043, #5183, #6264, .T. ) ;
#8829 = DIRECTION ( 'NONE',  ( 0.000000000000000000, 4.440892098500620738E-16, 1.000000000000000000 ) ) ;
#8830 = AXIS2_PLACEMENT_3D ( 'NONE', #12631, #8167, #11539 ) ;
#8831 = DIRECTION ( 'NONE',  ( 0.3822382184081047352, -0.9240638205168504316, -0.000000000000000000 ) ) ;
#8832 = CARTESIAN_POINT ( 'NONE',  ( 2.602085213965210642E-15, 5.773502691896274186, -6.000000000000005329 ) ) ;
#8833 = VECTOR ( 'NONE', #5523, 1000.000000000000000 ) ;
#8834 = CARTESIAN_POINT ( 'NONE',  ( 20.00000000000000355, 30.00000000000000711, 25.00000000000000000 ) ) ;
#8835 = VECTOR ( 'NONE', #13088, 1000.000000000000000 ) ;
#8836 = CARTESIAN_POINT ( 'NONE',  ( -140.0000000000003411, 189.5765550933606107, 47.99999999999998579 ) ) ;
#8837 = CARTESIAN_POINT ( 'NONE',  ( 4.132952817037849336, 2.031684012687273722, -3.518979934899746365 ) ) ;
#8838 = VERTEX_POINT ( 'NONE', #4018 ) ;
#8839 = DIRECTION ( 'NONE',  ( 0.000000000000000000, -1.000000000000000000, 0.000000000000000000 ) ) ;
#8840 = ORIENTED_EDGE ( 'NONE', *, *, #13785, .F. ) ;
#8841 = CIRCLE ( 'NONE', #9074, 2.500000000000002220 ) ;
#8842 = ORIENTED_EDGE ( 'NONE', *, *, #6189, .F. ) ;
#8843 = ORIENTED_EDGE ( 'NONE', *, *, #367, .T. ) ;
#8844 = CARTESIAN_POINT ( 'NONE',  ( 2.179555516819076999, -4.788648424347465848, -4.357628883416072796 ) ) ;
#8845 = CARTESIAN_POINT ( 'NONE',  ( 105.6817075744280743, 59.57655509336061073, -25.00000000000000000 ) ) ;
#8846 = DIRECTION ( 'NONE',  ( -0.2425356250363328581, 0.9701425001453318764, 0.000000000000000000 ) ) ;
#8847 = APPLICATION_CONTEXT ( 'automotive_design' ) ;
#8848 = CARTESIAN_POINT ( 'NONE',  ( 0.000000000000000000, 199.5765550933606107, -37.00000000000003553 ) ) ;
#8849 = CARTESIAN_POINT ( 'NONE',  ( 4.870920456765259310, 3.129869081975187761, -2.723603336645452622 ) ) ;
#8850 = CARTESIAN_POINT ( 'NONE',  ( 0.6666666666666679619, -4.233901974057278750, -3.000726591567075552 ) ) ;
#8851 = CARTESIAN_POINT ( 'NONE',  ( 0.000000000000000000, 0.000000000000000000, 0.000000000000000000 ) ) ;
#8852 = CARTESIAN_POINT ( 'NONE',  ( 31.38313257588138683, 143.6985259526510390, -28.00000000000000000 ) ) ;
#8853 = EDGE_LOOP ( 'NONE', ( #7623, #3678, #3075, #10575 ) ) ;
#8854 = DIRECTION ( 'NONE',  ( -1.000000000000000000, 0.000000000000000000, 0.000000000000000000 ) ) ;
#8855 = DIRECTION ( 'NONE',  ( 0.000000000000000000, -0.000000000000000000, -1.000000000000000000 ) ) ;
#8856 = LINE ( 'NONE', #5424, #2650 ) ;
#8857 = CARTESIAN_POINT ( 'NONE',  ( 59.18121602037099649, 13.58289998256015352, 25.00000000000000000 ) ) ;
#8858 = AXIS2_PLACEMENT_3D ( 'NONE', #2636, #3736, #1681 ) ;
#8859 = ADVANCED_FACE ( 'NONE', ( #4241 ), #6114, .T. ) ;
#8860 = CARTESIAN_POINT ( 'NONE',  ( -108.6817075744280743, 29.57655509336044020, -117.0000000000000000 ) ) ;
#8861 = ADVANCED_FACE ( 'NONE', ( #14120 ), #9776, .T. ) ;
#8862 = DIRECTION ( 'NONE',  ( 0.000000000000000000, 0.000000000000000000, 1.000000000000000000 ) ) ;
#8863 = AXIS2_PLACEMENT_3D ( 'NONE', #7160, #4130, #9595 ) ;
#8864 = CARTESIAN_POINT ( 'NONE',  ( 5.108706126686590743, 2.382237260725047712, 4.077515513881460052 ) ) ;
#8865 = EDGE_LOOP ( 'NONE', ( #8418, #9962, #6843, #2165, #2252 ) ) ;
#8866 = ORIENTED_EDGE ( 'NONE', *, *, #601, .T. ) ;
#8867 = CARTESIAN_POINT ( 'NONE',  ( 4.999999999999999112, -1.924500897298769608, -4.118275046351174140 ) ) ;
#8868 = AXIS2_PLACEMENT_3D ( 'NONE', #8795, #5435, #2073 ) ;
#8869 = ORIENTED_EDGE ( 'NONE', *, *, #10881, .T. ) ;
#8870 = DIRECTION ( 'NONE',  ( 1.000000000000000000, 0.000000000000000000, -2.081668171172168760E-16 ) ) ;
#8871 = EDGE_CURVE ( 'NONE', #1934, #9323, #2051, .T. ) ;
#8872 = CARTESIAN_POINT ( 'NONE',  ( 18.68170757442808849, 141.2731697022877313, -23.00000000000000000 ) ) ;
#8873 = ORIENTED_EDGE ( 'NONE', *, *, #4600, .T. ) ;
#8874 = VERTEX_POINT ( 'NONE', #3069 ) ;
#8875 = ADVANCED_FACE ( 'NONE', ( #6200 ), #4106, .F. ) ;
#8876 = PLANE ( 'NONE',  #10617 ) ;
#8877 = CARTESIAN_POINT ( 'NONE',  ( 76.68170757442801744, 39.57655509336063204, 33.00000000000000000 ) ) ;
#8878 = CARTESIAN_POINT ( 'NONE',  ( 4.052424581287747962, 2.393186648133197370, -2.990837702970422729 ) ) ;
#8879 = COLOUR_RGB ( '', 0.31764706, 0.68627451, 0.89019608) ;
#8880 = CARTESIAN_POINT ( 'NONE',  ( 22.00000000000000355, 47.00000000000000000, -25.00000000000000000 ) ) ;
#8881 = CIRCLE ( 'NONE', #11687, 5.499999999999976907 ) ;
#8882 = DIRECTION ( 'NONE',  ( 1.000000000000000000, 3.286707217423839940E-17, -2.273843122241290364E-18 ) ) ;
#8883 = SHAPE_REPRESENTATION ( 'torque nut 04-2_iso_ISO 7043-M5-N', ( #11025 ), #11250 ) ;
#8884 = CARTESIAN_POINT ( 'NONE',  ( -1.598077599628788370, 4.850852159564692734, -4.271474537231044977 ) ) ;
#8885 = ORIENTED_EDGE ( 'NONE', *, *, #7427, .F. ) ;
#8886 = LINE ( 'NONE', #13166, #9118 ) ;
#8887 = CARTESIAN_POINT ( 'NONE',  ( -3.357433326862111489, 3.835087656846199788, -0.07080520455421618342 ) ) ;
#8888 = CARTESIAN_POINT ( 'NONE',  ( 3.880206590543179512, 2.665671387532607906, 2.382921720510873254 ) ) ;
#8889 = EDGE_CURVE ( 'NONE', #10071, #9740, #13508, .T. ) ;
#8890 = AXIS2_PLACEMENT_3D ( 'NONE', #1991, #14216, #7531 ) ;
#8891 = VECTOR ( 'NONE', #4590, 1000.000000000000000 ) ;
#8892 = ORIENTED_EDGE ( 'NONE', *, *, #13785, .T. ) ;
#8893 = ORIENTED_EDGE ( 'NONE', *, *, #4971, .F. ) ;
#8894 = VECTOR ( 'NONE', #1489, 1000.000000000000000 ) ;
#8895 = VERTEX_POINT ( 'NONE', #10670 ) ;
#8896 = PLANE ( 'NONE',  #12011 ) ;
#8897 = EDGE_LOOP ( 'NONE', ( #7187, #6028, #10275, #877 ) ) ;
#8898 = ADVANCED_FACE ( 'NONE', ( #12781 ), #7366, .F. ) ;
#8899 = CYLINDRICAL_SURFACE ( 'NONE', #2105, 2.499999999999999112 ) ;
#8900 = CARTESIAN_POINT ( 'NONE',  ( 2.750000000000003553, 40.49999999999999289, 8.000000000000007105 ) ) ;
#8901 = DIRECTION ( 'NONE',  ( 0.9240638205168504316, 0.3822382184081047352, 0.000000000000000000 ) ) ;
#8902 = VECTOR ( 'NONE', #13478, 1000.000000000000000 ) ;
#8903 = LINE ( 'NONE', #7512, #13753 ) ;
#8904 = VECTOR ( 'NONE', #9135, 1000.000000000000000 ) ;
#8905 = LINE ( 'NONE', #11175, #14078 ) ;
#8906 = CONTEXT_DEPENDENT_SHAPE_REPRESENTATION ( #8493, #1329 ) ;
#8907 = DIRECTION ( 'NONE',  ( 0.000000000000000000, -8.482162385747133845E-47, 1.000000000000000000 ) ) ;
#8908 = CARTESIAN_POINT ( 'NONE',  ( 3.948103430090705857, -2.682758828852386923, 2.353325403973848484 ) ) ;
#8909 = ADVANCED_FACE ( 'NONE', ( #14187 ), #11988, .F. ) ;
#8910 = ADVANCED_FACE ( 'NONE', ( #847 ), #2931, .F. ) ;
#8911 = CARTESIAN_POINT ( 'NONE',  ( 4.082498951862935321, -2.020725942163680511, 3.499999999999991118 ) ) ;
#8912 = ORIENTED_EDGE ( 'NONE', *, *, #10296, .T. ) ;
#8913 = CIRCLE ( 'NONE', #12912, 2.500000000000002220 ) ;
#8914 = CIRCLE ( 'NONE', #246, 2.750000000000003997 ) ;
#8915 = CARTESIAN_POINT ( 'NONE',  ( 4.872112557122744825, -2.415761400130177830E-11, -4.072377784234180176 ) ) ;
#8916 = VERTEX_POINT ( 'NONE', #11842 ) ;
#8917 = ORIENTED_EDGE ( 'NONE', *, *, #607, .F. ) ;
#8918 = LINE ( 'NONE', #5550, #6371 ) ;
#8919 = DIRECTION ( 'NONE',  ( -1.000000000000000000, 0.000000000000000000, 0.000000000000000000 ) ) ;
#8920 = B_SPLINE_CURVE_WITH_KNOTS ( 'NONE', 3,
 ( #11920, #5321, #9784, #8688, #3148, #11168 ),
 .UNSPECIFIED., .F., .F.,
 ( 4, 2, 4 ),
 ( 0.002950759650825679654, 0.004429055062152274097, 0.005907350473478867672 ),
 .UNSPECIFIED. ) ;
#8921 = DIRECTION ( 'NONE',  ( 1.000000000000000000, 1.665334536937734071E-16, 0.000000000000000000 ) ) ;
#8922 = DIRECTION ( 'NONE',  ( -1.000000000000000000, 0.000000000000000000, 0.000000000000000000 ) ) ;
#8923 = DIRECTION ( 'NONE',  ( 1.000000000000000000, 1.665334536937734318E-16, 0.000000000000000000 ) ) ;
#8924 = DIRECTION ( 'NONE',  ( 0.000000000000000000, 0.000000000000000000, 1.000000000000000000 ) ) ;
#8925 = ORIENTED_EDGE ( 'NONE', *, *, #10049, .F. ) ;
#8926 = AXIS2_PLACEMENT_3D ( 'NONE', #9334, #9489, #12773 ) ;
#8927 = DIRECTION ( 'NONE',  ( 0.000000000000000000, 0.000000000000000000, 1.000000000000000000 ) ) ;
#8928 = ORIENTED_EDGE ( 'NONE', *, *, #13756, .T. ) ;
#8929 = AXIS2_PLACEMENT_3D ( 'NONE', #11860, #5197, #4190 ) ;
#8930 = DIRECTION ( 'NONE',  ( 0.000000000000000000, 0.000000000000000000, -1.000000000000000000 ) ) ;
#8931 = DIRECTION ( 'NONE',  ( 0.000000000000000000, 0.000000000000000000, 1.000000000000000000 ) ) ;
#8932 = DIRECTION ( 'NONE',  ( 0.000000000000000000, 4.440892098500620738E-16, 1.000000000000000000 ) ) ;
#8933 = LINE ( 'NONE', #13430, #13600 ) ;
#8934 = CIRCLE ( 'NONE', #7998, 2.500000000000002220 ) ;
#8935 = AXIS2_PLACEMENT_3D ( 'NONE', #8496, #10766, #11941 ) ;
#8936 = CARTESIAN_POINT ( 'NONE',  ( 19.99999999999999645, 67.00000000000000000, -25.00000000000000000 ) ) ;
#8937 = LINE ( 'NONE', #9820, #12531 ) ;
#8938 = FACE_OUTER_BOUND ( 'NONE', #6318, .T. ) ;
#8939 = B_SPLINE_CURVE_WITH_KNOTS ( 'NONE', 3,
 ( #2618, #7064, #9422, #8239 ),
 .UNSPECIFIED., .F., .F.,
 ( 4, 4 ),
 ( 2.380739282110561210E-07, 0.002044882221487530176 ),
 .UNSPECIFIED. ) ;
#8940 = CARTESIAN_POINT ( 'NONE',  ( 4.769971895851991661, -0.8344440309347370688, 4.000000000000002665 ) ) ;
#8941 = VERTEX_POINT ( 'NONE', #13092 ) ;
#8942 = FACE_OUTER_BOUND ( 'NONE', #3274, .T. ) ;
#8943 = CIRCLE ( 'NONE', #4535, 2.500000000000002220 ) ;
#8944 = EDGE_CURVE ( 'NONE', #5102, #12564, #13022, .T. ) ;
#8945 = SURFACE_STYLE_FILL_AREA ( #28 ) ;
#8946 = EDGE_CURVE ( 'NONE', #5022, #4126, #1815, .T. ) ;
#8947 = ORIENTED_EDGE ( 'NONE', *, *, #230, .T. ) ;
#8948 = PLANE ( 'NONE',  #4977 ) ;
#8949 = EDGE_CURVE ( 'NONE', #1753, #1352, #1119, .T. ) ;
#8950 = ORIENTED_EDGE ( 'NONE', *, *, #12096, .T. ) ;
#8951 = CARTESIAN_POINT ( 'NONE',  ( 2.749999999999997780, 25.49999999999996803, 0.000000000000000000 ) ) ;
#8952 = DIRECTION ( 'NONE',  ( 0.000000000000000000, 0.000000000000000000, -1.000000000000000000 ) ) ;
#8953 =( REPRESENTATION_RELATIONSHIP ('NONE','NONE', #10295, #852 ) REPRESENTATION_RELATIONSHIP_WITH_TRANSFORMATION ( #13244 )SHAPE_REPRESENTATION_RELATIONSHIP( ) );
#8954 = CARTESIAN_POINT ( 'NONE',  ( 129.3408537872138595, 189.5765550933606107, -75.00000000000001421 ) ) ;
#8955 = CARTESIAN_POINT ( 'NONE',  ( -3.349226789952651995, -2.685125164760746586, -0.2236248678334861184 ) ) ;
#8956 = CARTESIAN_POINT ( 'NONE',  ( 3.951447005078477126, 2.357513599190965259, -2.916666666666663854 ) ) ;
#8957 = EDGE_CURVE ( 'NONE', #8214, #13520, #6473, .T. ) ;
#8958 = PLANE ( 'NONE',  #12353 ) ;
#8959 = EDGE_LOOP ( 'NONE', ( #7269, #13474, #8869 ) ) ;
#8960 =( NAMED_UNIT ( * ) PLANE_ANGLE_UNIT ( ) SI_UNIT ( $, .RADIAN. ) );
#8961 = VECTOR ( 'NONE', #13691, 1000.000000000000000 ) ;
#8962 = VERTEX_POINT ( 'NONE', #8386 ) ;
#8963 = LINE ( 'NONE', #13232, #11651 ) ;
#8964 = ADVANCED_FACE ( 'NONE', ( #7296 ), #9764, .T. ) ;
#8965 = PLANE ( 'NONE',  #10452 ) ;
#8966 = AXIS2_PLACEMENT_3D ( 'NONE', #8104, #13845, #444 ) ;
#8967 = VERTEX_POINT ( 'NONE', #4397 ) ;
#8968 = ORIENTED_EDGE ( 'NONE', *, *, #13189, .F. ) ;
#8969 = VERTEX_POINT ( 'NONE', #9872 ) ;
#8970 = CONICAL_SURFACE ( 'NONE', #8025, 2.500000000000002220, 0.9599310885968781459 ) ;
#8971 = CARTESIAN_POINT ( 'NONE',  ( 0.3572655899080068309, -2.309401076758678339, -4.000000000000031086 ) ) ;
#8972 = ORIENTED_EDGE ( 'NONE', *, *, #8567, .T. ) ;
#8973 = CARTESIAN_POINT ( 'NONE',  ( 0.000000000000000000, 0.000000000000000000, -0.3501037691048258793 ) ) ;
#8974 = DIRECTION ( 'NONE',  ( 0.000000000000000000, 0.000000000000000000, 1.000000000000000000 ) ) ;
#8975 = CARTESIAN_POINT ( 'NONE',  ( 2.749999999999997780, 25.49999999999996803, 8.000000000000007105 ) ) ;
#8976 = ADVANCED_FACE ( 'NONE', ( #860, #14411 ), #8763, .T. ) ;
#8977 = DIRECTION ( 'NONE',  ( 0.000000000000000000, 1.000000000000000000, 0.000000000000000000 ) ) ;
#8978 = LINE ( 'NONE', #2326, #6547 ) ;
#8979 = CARTESIAN_POINT ( 'NONE',  ( -5.594483210025202879E-14, -5.773502691896268857, -0.5999999999999894307 ) ) ;
#8980 = DIRECTION ( 'NONE',  ( 0.000000000000000000, 0.000000000000000000, -1.000000000000000000 ) ) ;
#8981 = CARTESIAN_POINT ( 'NONE',  ( 22.00000000000000000, 78.00000000000000000, 25.00000000000000000 ) ) ;
#8982 = ORIENTED_EDGE ( 'NONE', *, *, #3008, .F. ) ;
#8983 = EDGE_LOOP ( 'NONE', ( #8066, #8047 ) ) ;
#8984 = LINE ( 'NONE', #4751, #6619 ) ;
#8985 = EDGE_LOOP ( 'NONE', ( #8332, #4296, #5512, #11367, #8471 ) ) ;
#8986 = ORIENTED_EDGE ( 'NONE', *, *, #13361, .F. ) ;
#8987 = CARTESIAN_POINT ( 'NONE',  ( 13.00000000000000533, 35.49999999999997158, 8.000000000000007105 ) ) ;
#8988 = DIRECTION ( 'NONE',  ( 0.000000000000000000, 0.000000000000000000, -1.000000000000000000 ) ) ;
#8989 = CARTESIAN_POINT ( 'NONE',  ( -5.000000000000000000, 3.082653260002450768, -4.588940887454125317 ) ) ;
#8990 = ADVANCED_FACE ( 'NONE', ( #9724 ), #14199, .T. ) ;
#8991 = CARTESIAN_POINT ( 'NONE',  ( 20.00000000000000000, 47.00000000000000000, -25.00000000000000000 ) ) ;
#8992 = CARTESIAN_POINT ( 'NONE',  ( 36.99999999999999289, 80.00000000000000000, -23.00000000000000000 ) ) ;
#8993 = CARTESIAN_POINT ( 'NONE',  ( 0.000000000000000000, 4.618802153517016507, -4.699999999999981526 ) ) ;
#8994 = DIRECTION ( 'NONE',  ( -4.664070103548417302E-16, 0.9242245927363028635, 0.3818493186865932754 ) ) ;
#8995 = DIRECTION ( 'NONE',  ( -0.2425356250363330801, 0.9701425001453319874, 0.000000000000000000 ) ) ;
#8996 = ORIENTED_EDGE ( 'NONE', *, *, #7698, .F. ) ;
#8997 = FACE_OUTER_BOUND ( 'NONE', #13568, .T. ) ;
#8998 = DIRECTION ( 'NONE',  ( -0.000000000000000000, 1.000000000000000000, -0.000000000000000000 ) ) ;
#8999 = VECTOR ( 'NONE', #3486, 1000.000000000000000 ) ;
#9000 = ORIENTED_EDGE ( 'NONE', *, *, #7298, .F. ) ;
#9001 = CARTESIAN_POINT ( 'NONE',  ( 56.75585977000769589, 23.28432498401347672, -25.00000000000000000 ) ) ;
#9002 = LINE ( 'NONE', #13494, #2854 ) ;
#9003 = ADVANCED_FACE ( 'NONE', ( #6420 ), #12068, .T. ) ;
#9004 = CYLINDRICAL_SURFACE ( 'NONE', #8858, 3.299999999999997158 ) ;
#9005 = EDGE_CURVE ( 'NONE', #5760, #6982, #929, .T. ) ;
#9006 =( NAMED_UNIT ( * ) SI_UNIT ( $, .STERADIAN. ) SOLID_ANGLE_UNIT ( ) );
#9007 = CARTESIAN_POINT ( 'NONE',  ( 5.005210039549695900, -2.400508349366352157, 4.000000000000003553 ) ) ;
#9008 = VERTEX_POINT ( 'NONE', #7650 ) ;
#9009 = ORIENTED_EDGE ( 'NONE', *, *, #2646, .F. ) ;
#9010 = FACE_OUTER_BOUND ( 'NONE', #5372, .T. ) ;
#9011 =( NAMED_UNIT ( * ) PLANE_ANGLE_UNIT ( ) SI_UNIT ( $, .RADIAN. ) );
#9012 = ORIENTED_EDGE ( 'NONE', *, *, #5664, .F. ) ;
#9013 = CARTESIAN_POINT ( 'NONE',  ( -4.000000000000001776, -1.762750951161524442E-16, 13.31572692736082786 ) ) ;
#9014 = ORIENTED_EDGE ( 'NONE', *, *, #6363, .T. ) ;
#9015 = PLANE ( 'NONE',  #5465 ) ;
#9016 = DIRECTION ( 'NONE',  ( 0.000000000000000000, 0.000000000000000000, -1.000000000000000000 ) ) ;
#9017 = CARTESIAN_POINT ( 'NONE',  ( 0.000000000000000000, 0.000000000000000000, 1.599999999999990319 ) ) ;
#9018 = DIRECTION ( 'NONE',  ( -2.273843122241288438E-18, -5.551115123125783935E-17, -1.000000000000000000 ) ) ;
#9019 = LINE ( 'NONE', #3628, #4429 ) ;
#9020 = FACE_OUTER_BOUND ( 'NONE', #6618, .T. ) ;
#9021 = ORIENTED_EDGE ( 'NONE', *, *, #7803, .F. ) ;
#9022 = DIRECTION ( 'NONE',  ( 1.000000000000000000, 0.000000000000000000, 0.000000000000000000 ) ) ;
#9023 = VERTEX_POINT ( 'NONE', #3289 ) ;
#9024 = CARTESIAN_POINT ( 'NONE',  ( -3.999999999999994671, -1.942223658245632256, -0.3516579909967634809 ) ) ;
#9025 = CARTESIAN_POINT ( 'NONE',  ( 3.950241966887836575, 2.668221755854076171, 2.378504353000507443 ) ) ;
#9026 = ORIENTED_EDGE ( 'NONE', *, *, #3260, .T. ) ;
#9027 = APPLICATION_CONTEXT ( 'automotive_design' ) ;
#9028 = EDGE_CURVE ( 'NONE', #14130, #375, #9938, .T. ) ;
#9029 = ORIENTED_EDGE ( 'NONE', *, *, #13681, .T. ) ;
#9030 = AXIS2_PLACEMENT_3D ( 'NONE', #6606, #12107, #5443 ) ;
#9031 = ORIENTED_EDGE ( 'NONE', *, *, #12048, .F. ) ;
#9032 = CIRCLE ( 'NONE', #4622, 0.5499999999999992673 ) ;
#9033 = CARTESIAN_POINT ( 'NONE',  ( 18.12748877629582367, 43.82334295289049919, 8.000000000000007105 ) ) ;
#9034 = VERTEX_POINT ( 'NONE', #3153 ) ;
#9035 = CARTESIAN_POINT ( 'NONE',  ( 4.071447262713911996, 2.020725942163681399, 3.499999999999996003 ) ) ;
#9036 = ADVANCED_FACE ( 'NONE', ( #1900 ), #3084, .T. ) ;
#9037 = CARTESIAN_POINT ( 'NONE',  ( 5.000000000000001776, 2.094482489769011302, -4.137545075662903749 ) ) ;
#9038 = ADVANCED_FACE ( 'NONE', ( #6351 ), #2037, .T. ) ;
#9039 = CARTESIAN_POINT ( 'NONE',  ( 33.99999999999998579, 80.00000000000000000, 25.00000000000000000 ) ) ;
#9040 = CARTESIAN_POINT ( 'NONE',  ( 19.99999999999999645, 57.00000000000000000, 25.00000000000000000 ) ) ;
#9041 = VERTEX_POINT ( 'NONE', #13180 ) ;
#9042 = DIRECTION ( 'NONE',  ( 1.000000000000000000, 0.000000000000000000, 0.000000000000000000 ) ) ;
#9043 = CONTEXT_DEPENDENT_SHAPE_REPRESENTATION ( #5750, #7990 ) ;
#9044 = DIRECTION ( 'NONE',  ( 0.000000000000000000, 0.000000000000000000, -1.000000000000000000 ) ) ;
#9045 = VECTOR ( 'NONE', #8289, 1000.000000000000000 ) ;
#9046 = CARTESIAN_POINT ( 'NONE',  ( 20.00000000000000000, 5.000000000000000000, -25.00000000000000000 ) ) ;
#9047 = CONICAL_SURFACE ( 'NONE', #3691, 6.438111078829122036, 1.221730476396037712 ) ;
#9048 = ORIENTED_EDGE ( 'NONE', *, *, #10476, .T. ) ;
#9049 = EDGE_CURVE ( 'NONE', #9323, #1934, #13519, .T. ) ;
#9050 = ORIENTED_EDGE ( 'NONE', *, *, #6173, .T. ) ;
#9051 = LINE ( 'NONE', #7955, #12466 ) ;
#9052 = EDGE_LOOP ( 'NONE', ( #5254, #13759, #3258, #585 ) ) ;
#9053 = CIRCLE ( 'NONE', #6731, 3.299999999999969624 ) ;
#9054 = ORIENTED_EDGE ( 'NONE', *, *, #3460, .T. ) ;
#9055 = AXIS2_PLACEMENT_3D ( 'NONE', #5676, #11458, #4605 ) ;
#9056 = CARTESIAN_POINT ( 'NONE',  ( -1.532072935877364915E-15, -6.066067634115591467, -4.659491423763650886 ) ) ;
#9057 = PLANE ( 'NONE',  #12410 ) ;
#9058 = LINE ( 'NONE', #11266, #5593 ) ;
#9059 = AXIS2_PLACEMENT_3D ( 'NONE', #13378, #8882, #2306 ) ;
#9060 = PLANE ( 'NONE',  #9116 ) ;
#9061 = EDGE_LOOP ( 'NONE', ( #5061, #7354, #10202, #11891, #11349, #4768, #13320 ) ) ;
#9062 = LINE ( 'NONE', #7, #1689 ) ;
#9063 = CARTESIAN_POINT ( 'NONE',  ( -125.4817075744280572, 109.5765550933604970, 7.815296581827839263E-15 ) ) ;
#9064 = CARTESIAN_POINT ( 'NONE',  ( 22.00000000000000355, 50.00000000000000000, 25.00000000000000000 ) ) ;
#9065 = ORIENTED_EDGE ( 'NONE', *, *, #11241, .F. ) ;
#9066 = EDGE_LOOP ( 'NONE', ( #2332, #11215 ) ) ;
#9067 = CIRCLE ( 'NONE', #10230, 2.000000000000001776 ) ;
#9068 = CARTESIAN_POINT ( 'NONE',  ( 0.3572655899081733644, -4.618802153516988973, -1.387778780781445676E-14 ) ) ;
#9069 = CIRCLE ( 'NONE', #9547, 10.00000000000000355 ) ;
#9070 = EDGE_CURVE ( 'NONE', #7329, #9244, #4628, .T. ) ;
#9071 = VERTEX_POINT ( 'NONE', #13242 ) ;
#9072 = CARTESIAN_POINT ( 'NONE',  ( 4.988724804725841011, 2.309401076758504701, -4.000000000000003553 ) ) ;
#9073 = CARTESIAN_POINT ( 'NONE',  ( -129.3408537872145132, 189.5765550933606107, -75.00000000000001421 ) ) ;
#9074 = AXIS2_PLACEMENT_3D ( 'NONE', #9186, #13683, #2542 ) ;
#9075 = ADVANCED_FACE ( 'NONE', ( #12133 ), #9047, .T. ) ;
#9076 = ORIENTED_EDGE ( 'NONE', *, *, #11989, .T. ) ;
#9077 = DIRECTION ( 'NONE',  ( -1.000000000000000000, 0.000000000000000000, 0.000000000000000000 ) ) ;
#9078 =( NAMED_UNIT ( * ) PLANE_ANGLE_UNIT ( ) SI_UNIT ( $, .RADIAN. ) );
#9079 = ORIENTED_EDGE ( 'NONE', *, *, #12048, .T. ) ;
#9080 = EDGE_CURVE ( 'NONE', #4403, #1350, #3217, .T. ) ;
#9081 = CARTESIAN_POINT ( 'NONE',  ( 0.000000000000000000, 0.000000000000000000, 13.31572692736082786 ) ) ;
#9082 = PRODUCT_RELATED_PRODUCT_CATEGORY ( 'part', '', ( #11275 ) ) ;
#9083 = EDGE_LOOP ( 'NONE', ( #450, #5844 ) ) ;
#9084 = ADVANCED_FACE ( 'NONE', ( #5472 ), #11871, .T. ) ;
#9085 = VECTOR ( 'NONE', #6131, 1000.000000000000000 ) ;
#9086 = ORIENTED_EDGE ( 'NONE', *, *, #5273, .T. ) ;
#9087 = UNCERTAINTY_MEASURE_WITH_UNIT (LENGTH_MEASURE( 1.000000000000000082E-05 ), #2368, 'distance_accuracy_value', 'NONE');
#9088 = DIRECTION ( 'NONE',  ( 0.000000000000000000, 0.000000000000000000, 1.000000000000000000 ) ) ;
#9089 = DIRECTION ( 'NONE',  ( 0.000000000000000000, 0.000000000000000000, -1.000000000000000000 ) ) ;
#9090 = ORIENTED_EDGE ( 'NONE', *, *, #6140, .F. ) ;
#9091 = CARTESIAN_POINT ( 'NONE',  ( 118.6817075744280316, 109.5765550933604828, 0.000000000000000000 ) ) ;
#9092 = CARTESIAN_POINT ( 'NONE',  ( 79.68170757442804586, 59.57655509336061073, 25.00000000000000000 ) ) ;
#9093 = CARTESIAN_POINT ( 'NONE',  ( 4.175813232069169878, 4.122719923832743660, 0.000000000000000000 ) ) ;
#9094 = CARTESIAN_POINT ( 'NONE',  ( 3.973514160553474284, 3.435084588004183814, -1.181876024140317671 ) ) ;
#9095 = ORIENTED_EDGE ( 'NONE', *, *, #2312, .T. ) ;
#9096 = CARTESIAN_POINT ( 'NONE',  ( 0.000000000000000000, 0.000000000000000000, 0.000000000000000000 ) ) ;
#9097 = B_SPLINE_CURVE_WITH_KNOTS ( 'NONE', 3,
 ( #1053, #2293, #11142, #4442, #6603 ),
 .UNSPECIFIED., .F., .F.,
 ( 4, 1, 4 ),
 ( 0.000000000000000000, 0.002020725942163690506, 0.004041451884327381013 ),
 .UNSPECIFIED. ) ;
#9098 = CARTESIAN_POINT ( 'NONE',  ( 19.99999999999999645, 57.00000000000000000, -25.00000000000000000 ) ) ;
#9099 = ORIENTED_EDGE ( 'NONE', *, *, #928, .F. ) ;
#9100 = CARTESIAN_POINT ( 'NONE',  ( 20.00000000000000355, 50.00000000000000000, -25.00000000000000000 ) ) ;
#9101 = ORIENTED_EDGE ( 'NONE', *, *, #7720, .F. ) ;
#9102 = ORIENTED_EDGE ( 'NONE', *, *, #10141, .F. ) ;
#9103 = EDGE_LOOP ( 'NONE', ( #11846, #13625 ) ) ;
#9104 = VECTOR ( 'NONE', #14392, 1000.000000000000000 ) ;
#9105 = CARTESIAN_POINT ( 'NONE',  ( 5.103531824934226080, -2.354098498486466351, -4.077418205400154427 ) ) ;
#9106 = ORIENTED_EDGE ( 'NONE', *, *, #1992, .F. ) ;
#9107 = CARTESIAN_POINT ( 'NONE',  ( 64.03192852109765454, -5.819950020346492892, -25.00000000000000000 ) ) ;
#9108 = CARTESIAN_POINT ( 'NONE',  ( 5.244936800657701070, -2.071448270550554138, -4.480299463185753339 ) ) ;
#9109 = CARTESIAN_POINT ( 'NONE',  ( 33.99999999999998579, 80.00000000000000000, -25.00000000000000000 ) ) ;
#9110 = CARTESIAN_POINT ( 'NONE',  ( 20.00000000000000000, 78.00000000000000000, -25.00000000000000000 ) ) ;
#9111 = ORIENTED_EDGE ( 'NONE', *, *, #3613, .T. ) ;
#9112 = B_SPLINE_CURVE_WITH_KNOTS ( 'NONE', 3,
 ( #8767, #3221, #12287, #13403, #12359, #7654, #3375, #13536, #6782, #2404, #14414, #1157, #11255, #10083, #6862, #12137 ),
 .UNSPECIFIED., .F., .F.,
 ( 4, 3, 3, 3, 3, 4 ),
 ( -2.214559098546004647E-06, 0.000000000000000000, 3.881464059292318041E-05, 7.921402936568111498E-05, 0.0001155901529638586709, 0.0001522174276056075621 ),
 .UNSPECIFIED. ) ;
#9113 = DIRECTION ( 'NONE',  ( -1.000000000000000000, 0.000000000000000000, 0.000000000000000000 ) ) ;
#9114 = CARTESIAN_POINT ( 'NONE',  ( -3.081487911019577365E-30, 3.469446951953614189E-15, -5.624496230895170257 ) ) ;
#9115 = CARTESIAN_POINT ( 'NONE',  ( 20.00000000000000355, 40.00000000000000711, 25.00000000000000000 ) ) ;
#9116 = AXIS2_PLACEMENT_3D ( 'NONE', #7079, #8101, #13629 ) ;
#9117 = DIRECTION ( 'NONE',  ( 0.000000000000000000, 0.000000000000000000, 1.000000000000000000 ) ) ;
#9118 = VECTOR ( 'NONE', #4528, 1000.000000000000000 ) ;
#9119 = CIRCLE ( 'NONE', #5623, 2.600000000000004974 ) ;
#9120 = EDGE_CURVE ( 'NONE', #3642, #10492, #8903, .T. ) ;
#9121 = ORIENTED_EDGE ( 'NONE', *, *, #11968, .F. ) ;
#9122 = DIRECTION ( 'NONE',  ( -0.000000000000000000, -0.000000000000000000, -1.000000000000000000 ) ) ;
#9123 = ORIENTED_EDGE ( 'NONE', *, *, #2501, .F. ) ;
#9124 = CIRCLE ( 'NONE', #12181, 2.749999999999997780 ) ;
#9125 = ORIENTED_EDGE ( 'NONE', *, *, #4235, .F. ) ;
#9126 = CARTESIAN_POINT ( 'NONE',  ( -108.6817075744280743, 29.57655509336044020, 33.00000000000002842 ) ) ;
#9127 = COLOUR_RGB ( '', 0.31764706, 0.68627451, 0.89019608) ;
#9128 = CARTESIAN_POINT ( 'NONE',  ( 0.3126073911696169993, -2.020725942163681399, 3.499999999999989342 ) ) ;
#9129 = LINE ( 'NONE', #4755, #223 ) ;
#9130 = CIRCLE ( 'NONE', #503, 2.750000000000003997 ) ;
#9131 = CARTESIAN_POINT ( 'NONE',  ( 2.345747346278098888, -3.264484291692517193, -0.01223254789874875237 ) ) ;
#9132 = LINE ( 'NONE', #13844, #14300 ) ;
#9133 = CARTESIAN_POINT ( 'NONE',  ( 0.000000000000000000, 0.000000000000000000, 0.000000000000000000 ) ) ;
#9134 = EDGE_CURVE ( 'NONE', #32, #10813, #13397, .T. ) ;
#9135 = DIRECTION ( 'NONE',  ( 0.000000000000000000, 0.000000000000000000, 1.000000000000000000 ) ) ;
#9137 = ORIENTED_EDGE ( 'NONE', *, *, #747, .F. ) ;
#9136 = B_SPLINE_CURVE_WITH_KNOTS ( 'NONE', 3,
 ( #10887, #12066, #13105, #6480, #4254, #11998 ),
 .UNSPECIFIED., .F., .F.,
 ( 4, 2, 4 ),
 ( 0.003058795990767210031, 0.004586520967003277979, 0.006114245943239346795 ),
 .UNSPECIFIED. ) ;
#9138 = AXIS2_PLACEMENT_3D ( 'NONE', #7876, #930, #6779 ) ;
#9139 = MECHANICAL_DESIGN_GEOMETRIC_PRESENTATION_REPRESENTATION (  '', ( #2852 ), #1201 ) ;
#9140 = CARTESIAN_POINT ( 'NONE',  ( 2.500000000000011546, -4.330127018922186544, 0.000000000000000000 ) ) ;
#9141 = EDGE_CURVE ( 'NONE', #3184, #7502, #1976, .T. ) ;
#9142 = VERTEX_POINT ( 'NONE', #11249 ) ;
#9143 = ORIENTED_EDGE ( 'NONE', *, *, #4681, .T. ) ;
#9144 = EDGE_LOOP ( 'NONE', ( #14277, #7942 ) ) ;
#9145 = ORIENTED_EDGE ( 'NONE', *, *, #11014, .T. ) ;
#9146 = CARTESIAN_POINT ( 'NONE',  ( -2.000000000000001776, 3.464101615137757495, 0.000000000000000000 ) ) ;
#9147 = CARTESIAN_POINT ( 'NONE',  ( 22.00000000000000000, 67.00000000000000000, 25.00000000000000000 ) ) ;
#9148 = AXIS2_PLACEMENT_3D ( 'NONE', #9173, #8290, #8367 ) ;
#9149 = VECTOR ( 'NONE', #5812, 1000.000000000000000 ) ;
#9150 = CIRCLE ( 'NONE', #2386, 2.699999999999999289 ) ;
#9151 = EDGE_CURVE ( 'NONE', #4271, #7272, #11386, .T. ) ;
#9152 = ORIENTED_EDGE ( 'NONE', *, *, #5295, .F. ) ;
#9153 = ORIENTED_EDGE ( 'NONE', *, *, #747, .T. ) ;
#9154 = CYLINDRICAL_SURFACE ( 'NONE', #2058, 5.000000000000004441 ) ;
#9155 = CARTESIAN_POINT ( 'NONE',  ( -2.000000000000001776, 3.464101615137757495, 0.000000000000000000 ) ) ;
#9156 = ORIENTED_EDGE ( 'NONE', *, *, #6576, .F. ) ;
#9157 = DIRECTION ( 'NONE',  ( 0.000000000000000000, 0.000000000000000000, 1.000000000000000000 ) ) ;
#9158 = AXIS2_PLACEMENT_3D ( 'NONE', #9591, #10541, #13041 ) ;
#9159 = AXIS2_PLACEMENT_3D ( 'NONE', #6292, #5276, #10694 ) ;
#9160 = PRODUCT_DEFINITION_SHAPE ( 'NONE', 'NONE',  #14474 ) ;
#9161 = DIRECTION ( 'NONE',  ( 0.000000000000000000, 0.000000000000000000, 1.000000000000000000 ) ) ;
#9162 = CARTESIAN_POINT ( 'NONE',  ( 4.165266963751697915, 2.049631966911992009, 3.550066703508893529 ) ) ;
#9163 = PLANE ( 'NONE',  #2343 ) ;
#9164 = DIRECTION ( 'NONE',  ( -1.000000000000000000, -1.665334536937734071E-16, 0.000000000000000000 ) ) ;
#9165 = FACE_OUTER_BOUND ( 'NONE', #1386, .T. ) ;
#9166 = EDGE_CURVE ( 'NONE', #7617, #11427, #5086, .T. ) ;
#9167 = CARTESIAN_POINT ( 'NONE',  ( 19.99999999999999645, 67.00000000000000000, -25.00000000000000000 ) ) ;
#9168 = CIRCLE ( 'NONE', #3352, 3.000000000000003553 ) ;
#9169 = ORIENTED_EDGE ( 'NONE', *, *, #205, .F. ) ;
#9170 = FACE_OUTER_BOUND ( 'NONE', #11117, .T. ) ;
#9171 = ORIENTED_EDGE ( 'NONE', *, *, #4900, .F. ) ;
#9172 = LINE ( 'NONE', #9098, #1367 ) ;
#9173 = CARTESIAN_POINT ( 'NONE',  ( 78.52142056027061301, -86.08568224108226730, -28.00000000000000000 ) ) ;
#9174 = ORIENTED_EDGE ( 'NONE', *, *, #9224, .F. ) ;
#9175 = DIRECTION ( 'NONE',  ( -1.000000000000000000, 0.000000000000000000, 0.000000000000000000 ) ) ;
#9176 = EDGE_LOOP ( 'NONE', ( #3135, #12375, #8019, #8005 ) ) ;
#9177 = EDGE_LOOP ( 'NONE', ( #8286, #11091, #13236, #13999 ) ) ;
#9178 = VECTOR ( 'NONE', #3634, 1000.000000000000000 ) ;
#9179 = ORIENTED_EDGE ( 'NONE', *, *, #12406, .F. ) ;
#9180 = FACE_OUTER_BOUND ( 'NONE', #9896, .T. ) ;
#9181 = DIRECTION ( 'NONE',  ( 0.000000000000000000, 0.000000000000000000, -1.000000000000000000 ) ) ;
#9182 = EDGE_LOOP ( 'NONE', ( #3450, #4982 ) ) ;
#9183 = CARTESIAN_POINT ( 'NONE',  ( 2.344047193898593839, 3.265465875126470241, -5.393482291641755831E-15 ) ) ;
#9184 = CIRCLE ( 'NONE', #561, 2.500000000000002220 ) ;
#9185 = CARTESIAN_POINT ( 'NONE',  ( 5.000000000000000888, -3.082649547295097658, -4.588940179250877271 ) ) ;
#9186 = CARTESIAN_POINT ( 'NONE',  ( 49.47979101891770171, 52.38859998837343568, 25.00000000000000000 ) ) ;
#9187 = EDGE_CURVE ( 'NONE', #10652, #6291, #3471, .T. ) ;
#9188 = CARTESIAN_POINT ( 'NONE',  ( -4.211140560182201398, -2.431303136016548017, -3.445885042887453231 ) ) ;
#9189 = EDGE_CURVE ( 'NONE', #181, #777, #66, .T. ) ;
#9190 = ORIENTED_EDGE ( 'NONE', *, *, #429, .F. ) ;
#9191 = CARTESIAN_POINT ( 'NONE',  ( 22.00000000000000355, 50.00000000000000000, -25.00000000000000000 ) ) ;
#9192 = PRODUCT_RELATED_PRODUCT_CATEGORY ( 'part', '', ( #11629 ) ) ;
#9193 = LINE ( 'NONE', #352, #2124 ) ;
#9194 = CARTESIAN_POINT ( 'NONE',  ( 0.03421028094653593560, 3.072372537026365702, -2.678494666091054022 ) ) ;
#9195 = CARTESIAN_POINT ( 'NONE',  ( 5.000000000000000888, 0.000000000000000000, 0.000000000000000000 ) ) ;
#9196 = EDGE_CURVE ( 'NONE', #5064, #2621, #11173, .T. ) ;
#9197 = AXIS2_PLACEMENT_3D ( 'NONE', #7991, #3557, #2442 ) ;
#9198 = ORIENTED_EDGE ( 'NONE', *, *, #10840, .F. ) ;
#9199 = ORIENTED_EDGE ( 'NONE', *, *, #7156, .F. ) ;
#9200 = CARTESIAN_POINT ( 'NONE',  ( 20.00000000000000000, 70.00000000000000000, -25.00000000000000000 ) ) ;
#9201 = ORIENTED_EDGE ( 'NONE', *, *, #13931, .F. ) ;
#9202 = ORIENTED_EDGE ( 'NONE', *, *, #5080, .T. ) ;
#9203 = DIRECTION ( 'NONE',  ( -0.9701425001453318764, -0.2425356250363329969, 0.000000000000000000 ) ) ;
#9204 = CARTESIAN_POINT ( 'NONE',  ( 8.000000000000000000, 25.49999999999996803, 8.000000000000007105 ) ) ;
#9205 = DIRECTION ( 'NONE',  ( 0.000000000000000000, 0.000000000000000000, 1.000000000000000000 ) ) ;
#9206 = DIRECTION ( 'NONE',  ( 5.493715166364590271E-32, -0.8660254037844383745, -0.5000000000000005551 ) ) ;
#9207 = ADVANCED_FACE ( 'NONE', ( #9263 ), #3649, .T. ) ;
#9208 = DIRECTION ( 'NONE',  ( 0.000000000000000000, 0.000000000000000000, 1.000000000000000000 ) ) ;
#9209 = CARTESIAN_POINT ( 'NONE',  ( -1.343349931607518297E-17, 40.49999999999999289, -45.69999999999998153 ) ) ;
#9210 = EDGE_CURVE ( 'NONE', #8874, #6118, #13983, .T. ) ;
#9211 = CARTESIAN_POINT ( 'NONE',  ( 20.00000000000000355, 50.00000000000000000, 25.00000000000000000 ) ) ;
#9212 = EDGE_CURVE ( 'NONE', #3878, #14186, #13280, .T. ) ;
#9213 = ORIENTED_EDGE ( 'NONE', *, *, #3008, .T. ) ;
#9214 = CARTESIAN_POINT ( 'NONE',  ( 61.53192852109764743, -5.819950020346492892, 25.00000000000000000 ) ) ;
#9215 = EDGE_LOOP ( 'NONE', ( #11644, #7343 ) ) ;
#9216 = ORIENTED_EDGE ( 'NONE', *, *, #3530, .F. ) ;
#9217 = EDGE_LOOP ( 'NONE', ( #9179, #12941, #9567, #12103, #8479 ) ) ;
#9218 = EDGE_CURVE ( 'NONE', #11189, #5462, #2400, .T. ) ;
#9219 = PRODUCT_DEFINITION_CONTEXT ( 'detailed design', #12885, 'design' ) ;
#9220 = EDGE_LOOP ( 'NONE', ( #7620, #7024, #8917, #9754 ) ) ;
#9221 = CARTESIAN_POINT ( 'NONE',  ( -2.855764796983338183, 2.970025579236424740, -0.09382832055446015118 ) ) ;
#9222 = DIRECTION ( 'NONE',  ( 0.000000000000000000, 0.000000000000000000, -1.000000000000000000 ) ) ;
#9223 = EDGE_CURVE ( 'NONE', #11164, #6869, #6952, .T. ) ;
#9224 = EDGE_CURVE ( 'NONE', #10181, #12327, #1438, .T. ) ;
#9225 = EDGE_LOOP ( 'NONE', ( #1634, #211, #6647, #9860 ) ) ;
#9226 =( REPRESENTATION_RELATIONSHIP ('NONE','NONE', #10295, #8883 ) REPRESENTATION_RELATIONSHIP_WITH_TRANSFORMATION ( #8237 )SHAPE_REPRESENTATION_RELATIONSHIP( ) );
#9227 = EDGE_CURVE ( 'NONE', #8545, #13907, #10369, .T. ) ;
#9228 = ORIENTED_EDGE ( 'NONE', *, *, #1617, .F. ) ;
#9229 = DIRECTION ( 'NONE',  ( 0.000000000000000000, 0.000000000000000000, -1.000000000000000000 ) ) ;
#9230 = PLANE ( 'NONE',  #3569 ) ;
#9231 = ORIENTED_EDGE ( 'NONE', *, *, #14175, .T. ) ;
#9232 = LINE ( 'NONE', #10338, #1956 ) ;
#9233 = ORIENTED_EDGE ( 'NONE', *, *, #11083, .T. ) ;
#9234 = ADVANCED_FACE ( 'NONE', ( #13747 ), #6857, .F. ) ;
#9235 = UNCERTAINTY_MEASURE_WITH_UNIT (LENGTH_MEASURE( 1.000000000000000082E-05 ), #11658, 'distance_accuracy_value', 'NONE');
#9236 = CARTESIAN_POINT ( 'NONE',  ( 0.000000000000000000, -3.031088913245549854, -1.750000000000001554 ) ) ;
#9237 = CARTESIAN_POINT ( 'NONE',  ( 4.175572532730950748, 2.061029303918053834, 3.569807470274371397 ) ) ;
#9238 = ORIENTED_EDGE ( 'NONE', *, *, #11467, .T. ) ;
#9239 = DIRECTION ( 'NONE',  ( 0.000000000000000000, 0.000000000000000000, 1.000000000000000000 ) ) ;
#9240 = CARTESIAN_POINT ( 'NONE',  ( 71.80728622811317052, -17.99808865627607801, -25.00000000000000000 ) ) ;
#9241 = FILL_AREA_STYLE ('',( #10263 ) ) ;
#9242 = CARTESIAN_POINT ( 'NONE',  ( 3.514986608502523868, 4.017641317387379729, -4.357689166958453875 ) ) ;
#9243 = DIRECTION ( 'NONE',  ( 0.000000000000000000, 0.000000000000000000, 1.000000000000000000 ) ) ;
#9244 = VERTEX_POINT ( 'NONE', #6704 ) ;
#9245 = CYLINDRICAL_SURFACE ( 'NONE', #263, 2.100000000000000977 ) ;
#9246 = ORIENTED_EDGE ( 'NONE', *, *, #12210, .F. ) ;
#9247 = CARTESIAN_POINT ( 'NONE',  ( -3.999999999999995559, -0.7890432684750890990, -0.04868663549882130265 ) ) ;
#9248 = PLANE ( 'NONE',  #9148 ) ;
#9249 = ORIENTED_EDGE ( 'NONE', *, *, #4352, .T. ) ;
#9250 = CARTESIAN_POINT ( 'NONE',  ( 4.939003118777103296, -4.265486753575247647, -0.6119602237977784798 ) ) ;
#9251 = DIRECTION ( 'NONE',  ( 0.000000000000000000, 0.000000000000000000, -1.000000000000000000 ) ) ;
#9252 = ORIENTED_EDGE ( 'NONE', *, *, #9530, .F. ) ;
#9253 = DIRECTION ( 'NONE',  ( 0.000000000000000000, 1.000000000000000000, 0.000000000000000000 ) ) ;
#9254 = ORIENTED_EDGE ( 'NONE', *, *, #130, .T. ) ;
#9255 = ADVANCED_FACE ( 'NONE', ( #10287 ), #2325, .F. ) ;
#9256 = ORIENTED_EDGE ( 'NONE', *, *, #10690, .F. ) ;
#9257 = CARTESIAN_POINT ( 'NONE',  ( 42.20372226782770753, 81.49287499273339108, 25.00000000000000000 ) ) ;
#9258 = CARTESIAN_POINT ( 'NONE',  ( -0.6666666666666671848, -4.233901974057272533, -3.000726591567075996 ) ) ;
#9259 = VERTEX_POINT ( 'NONE', #9040 ) ;
#9260 = FACE_OUTER_BOUND ( 'NONE', #9651, .T. ) ;
#9261 = DIRECTION ( 'NONE',  ( -1.000000000000000000, 0.000000000000000000, 0.000000000000000000 ) ) ;
#9262 = FACE_OUTER_BOUND ( 'NONE', #12128, .T. ) ;
#9263 = FACE_OUTER_BOUND ( 'NONE', #10121, .T. ) ;
#9264 =( NAMED_UNIT ( * ) SI_UNIT ( $, .STERADIAN. ) SOLID_ANGLE_UNIT ( ) );
#9265 = CARTESIAN_POINT ( 'NONE',  ( 61.60657227073433262, 3.881474981106830313, 25.00000000000000000 ) ) ;
#9266 = DIRECTION ( 'NONE',  ( 1.000000000000000000, 1.665334536937734071E-16, 0.000000000000000000 ) ) ;
#9267 = FACE_OUTER_BOUND ( 'NONE', #8112, .T. ) ;
#9268 = AXIS2_PLACEMENT_3D ( 'NONE', #6308, #2966, #8279 ) ;
#9269 = LINE ( 'NONE', #355, #434 ) ;
#9270 = EDGE_LOOP ( 'NONE', ( #6407, #2425, #11756 ) ) ;
#9271 = B_SPLINE_CURVE_WITH_KNOTS ( 'NONE', 3,
 ( #10487, #12471, #247, #8060, #13795, #6897, #1274, #3485, #323, #11432, #10261, #2444, #2669, #11361, #5934, #13721 ),
 .UNSPECIFIED., .F., .F.,
 ( 4, 3, 3, 3, 3, 4 ),
 ( -2.111273352609310095E-06, 0.000000000000000000, 3.519286887794623349E-05, 7.191842652066866262E-05, 0.0001049868727093422117, 0.0001382836236821615838 ),
 .UNSPECIFIED. ) ;
#9272 = ORIENTED_EDGE ( 'NONE', *, *, #3842, .F. ) ;
#9273 = ADVANCED_FACE ( 'NONE', ( #3506 ), #11321, .T. ) ;
#9274 = PRODUCT_DEFINITION ( 'UNKNOWN', '', #12014, #7607 ) ;
#9275 = EDGE_CURVE ( 'NONE', #13954, #131, #198, .T. ) ;
#9276 = EDGE_LOOP ( 'NONE', ( #9050, #13679, #10092, #11021, #7958, #10298, #3315, #7867, #2690 ) ) ;
#9277 = B_SPLINE_CURVE_WITH_KNOTS ( 'NONE', 3,
 ( #6266, #7368, #5317, #1750, #11843, #1817, #5179, #1966 ),
 .UNSPECIFIED., .F., .F.,
 ( 4, 2, 2, 4 ),
 ( 2.465131517015980755E-07, 0.001183067374689848478, 0.001774477805458921998, 0.002365888236227995517 ),
 .UNSPECIFIED. ) ;
#9278 = CARTESIAN_POINT ( 'NONE',  ( 4.000000000000003553, -2.309401076758511806, -0.5000000000000004441 ) ) ;
#9279 = ORIENTED_EDGE ( 'NONE', *, *, #4936, .F. ) ;
#9280 = VERTEX_POINT ( 'NONE', #9110 ) ;
#9281 = CARTESIAN_POINT ( 'NONE',  ( 20.00000000000000000, 37.00000000000000711, -25.00000000000000000 ) ) ;
#9282 = CARTESIAN_POINT ( 'NONE',  ( 5.253368672218638125, 3.033033817057769532, -4.659491423763650886 ) ) ;
#9283 = DIRECTION ( 'NONE',  ( 1.734723475976770502E-18, -4.440892098500621231E-16, -1.000000000000000000 ) ) ;
#9284 = DIRECTION ( 'NONE',  ( 1.000000000000000000, 1.665334536937734071E-16, 0.000000000000000000 ) ) ;
#9285 = LINE ( 'NONE', #6874, #6808 ) ;
#9286 = AXIS2_PLACEMENT_3D ( 'NONE', #10997, #8739, #6528 ) ;
#9287 = FACE_BOUND ( 'NONE', #5697, .T. ) ;
#9288 = DIRECTION ( 'NONE',  ( 0.000000000000000000, 0.000000000000000000, -1.000000000000000000 ) ) ;
#9289 = CARTESIAN_POINT ( 'NONE',  ( 0.000000000000000000, 199.5765550933606107, -32.00000000000002842 ) ) ;
#9290 = CARTESIAN_POINT ( 'NONE',  ( 3.822382184081048351, 49.74063820516850143, 0.000000000000000000 ) ) ;
#9291 = VERTEX_POINT ( 'NONE', #13609 ) ;
#9292 = CARTESIAN_POINT ( 'NONE',  ( 4.071447262713911996, 4.041451884327390331, 0.000000000000000000 ) ) ;
#9293 = ORIENTED_EDGE ( 'NONE', *, *, #5383, .T. ) ;
#9294 = AXIS2_PLACEMENT_3D ( 'NONE', #13360, #5509, #10859 ) ;
#9295 = AXIS2_PLACEMENT_3D ( 'NONE', #1585, #4958, #1520 ) ;
#9296 = VERTEX_POINT ( 'NONE', #8018 ) ;
#9297 = EDGE_LOOP ( 'NONE', ( #8138, #634, #9642, #13328 ) ) ;
#9298 = CARTESIAN_POINT ( 'NONE',  ( -3.999999999999996447, 2.309401076758494487, -0.5000000000000004441 ) ) ;
#9299 = LINE ( 'NONE', #13780, #4708 ) ;
#9300 = AXIS2_PLACEMENT_3D ( 'NONE', #12837, #10413, #6007 ) ;
#9301 = VECTOR ( 'NONE', #4133, 999.9999999999998863 ) ;
#9302 = ORIENTED_EDGE ( 'NONE', *, *, #13450, .T. ) ;
#9303 = AXIS2_PLACEMENT_3D ( 'NONE', #1065, #13447, #117 ) ;
#9304 = ORIENTED_EDGE ( 'NONE', *, *, #8566, .T. ) ;
#9305 = DIRECTION ( 'NONE',  ( 1.000000000000000000, 0.000000000000000000, -0.000000000000000000 ) ) ;
#9306 = DIRECTION ( 'NONE',  ( 0.000000000000000000, 0.000000000000000000, -1.000000000000000000 ) ) ;
#9307 = VERTEX_POINT ( 'NONE', #9188 ) ;
#9308 = FACE_BOUND ( 'NONE', #12962, .T. ) ;
#9309 = EDGE_CURVE ( 'NONE', #11268, #13323, #12706, .T. ) ;
#9310 = CONICAL_SURFACE ( 'NONE', #11182, 4.000000000000004441, 1.047197551196600296 ) ;
#9311 = CARTESIAN_POINT ( 'NONE',  ( 3.370256023960729782E-15, 5.773502691896274186, -6.000000000000005329 ) ) ;
#9312 = CARTESIAN_POINT ( 'NONE',  ( -88.22284556172398595, 39.57655509336048283, 33.00000000000002842 ) ) ;
#9313 = DIRECTION ( 'NONE',  ( 1.000000000000000000, 0.000000000000000000, 0.000000000000000000 ) ) ;
#9314 = CARTESIAN_POINT ( 'NONE',  ( 5.733169058567799681, -6.938893903907228378E-15, 0.000000000000000000 ) ) ;
#9315 = FILL_AREA_STYLE_COLOUR ( '', #11991 ) ;
#9316 = DIRECTION ( 'NONE',  ( -1.000000000000000000, 0.000000000000000000, 0.000000000000000000 ) ) ;
#9317 = FACE_OUTER_BOUND ( 'NONE', #1674, .T. ) ;
#9318 = VERTEX_POINT ( 'NONE', #7210 ) ;
#9319 = CARTESIAN_POINT ( 'NONE',  ( 88.22284556172388648, 29.57655509336062849, 28.00000000000000000 ) ) ;
#9320 = CARTESIAN_POINT ( 'NONE',  ( -3.999999999999996447, -0.3979232138631241811, 1.502636448429128999E-15 ) ) ;
#9321 = EDGE_CURVE ( 'NONE', #5022, #13659, #2694, .T. ) ;
#9322 = CARTESIAN_POINT ( 'NONE',  ( -3.999999999999996447, -3.469446951953614189E-15, 0.000000000000000000 ) ) ;
#9323 = VERTEX_POINT ( 'NONE', #1812 ) ;
#9324 = CARTESIAN_POINT ( 'NONE',  ( 4.870920456765268192, -3.923644220354688184, -1.348744467187204199 ) ) ;
#9325 = FACE_OUTER_BOUND ( 'NONE', #4798, .T. ) ;
#9326 = MECHANICAL_DESIGN_GEOMETRIC_PRESENTATION_REPRESENTATION (  '', ( #3974 ), #10967 ) ;
#9328 = ORIENTED_EDGE ( 'NONE', *, *, #12817, .T. ) ;
#9327 = EDGE_CURVE ( 'NONE', #6578, #9071, #9067, .T. ) ;
#9329 = CARTESIAN_POINT ( 'NONE',  ( 5.084394237955924822, 4.671926501058326409, -1.387778780781445676E-14 ) ) ;
#9330 = VERTEX_POINT ( 'NONE', #1744 ) ;
#9331 = ORIENTED_EDGE ( 'NONE', *, *, #7881, .F. ) ;
#9332 = VERTEX_POINT ( 'NONE', #8235 ) ;
#9333 = DIRECTION ( 'NONE',  ( 0.000000000000000000, -0.000000000000000000, -1.000000000000000000 ) ) ;
#9334 = CARTESIAN_POINT ( 'NONE',  ( -28.00000000000000355, 29.99999999999999645, 0.000000000000000000 ) ) ;
#9335 = DIRECTION ( 'NONE',  ( -1.000000000000000000, 0.000000000000000000, 0.000000000000000000 ) ) ;
#9336 =( GEOMETRIC_REPRESENTATION_CONTEXT ( 3 ) GLOBAL_UNCERTAINTY_ASSIGNED_CONTEXT ( ( #8508 ) ) GLOBAL_UNIT_ASSIGNED_CONTEXT ( ( #7132, #11680, #8302 ) ) REPRESENTATION_CONTEXT ( 'NONE', 'WORKASPACE' ) );
#9337 = LINE ( 'NONE', #714, #1325 ) ;
#9338 = CARTESIAN_POINT ( 'NONE',  ( 4.158806752148098695, -2.089318365061883842, 3.499999999999993783 ) ) ;
#9339 = CARTESIAN_POINT ( 'NONE',  ( 2.749999999999997780, 25.49999999999996803, 8.000000000000007105 ) ) ;
#9340 = CARTESIAN_POINT ( 'NONE',  ( 3.822382184081048351, 49.74063820516850143, 8.000000000000007105 ) ) ;
#9341 = CARTESIAN_POINT ( 'NONE',  ( 5.000000000000000000, -2.886751345948148639, -4.284345921091780696 ) ) ;
#9342 = EDGE_CURVE ( 'NONE', #3727, #172, #12959, .T. ) ;
#9343 = FACE_OUTER_BOUND ( 'NONE', #13915, .T. ) ;
#9344 = CARTESIAN_POINT ( 'NONE',  ( -3.999999999999996447, 2.309401076758494487, -3.133295621305376422 ) ) ;
#9345 = VECTOR ( 'NONE', #6048, 999.9999999999998863 ) ;
#9346 = EDGE_CURVE ( 'NONE', #1507, #651, #3946, .T. ) ;
#9347 = ORIENTED_EDGE ( 'NONE', *, *, #12620, .T. ) ;
#9348 = LINE ( 'NONE', #13834, #6853 ) ;
#9349 = EDGE_LOOP ( 'NONE', ( #10748, #2202, #3282, #11242 ) ) ;
#9350 = ORIENTED_EDGE ( 'NONE', *, *, #1244, .F. ) ;
#9351 = DIRECTION ( 'NONE',  ( 1.000000000000000000, -2.551526159633733968E-19, -1.987661601597216239E-18 ) ) ;
#9352 = CARTESIAN_POINT ( 'NONE',  ( 0.2174200650117466826, -2.185595227304854227, 3.214438021527920686 ) ) ;
#9353 = DIRECTION ( 'NONE',  ( 0.000000000000000000, 0.000000000000000000, -1.000000000000000000 ) ) ;
#9354 = LINE ( 'NONE', #595, #704 ) ;
#9355 = CARTESIAN_POINT ( 'NONE',  ( -118.6817075744279606, -30.42344490663958112, 33.00000000000002842 ) ) ;
#9356 = CIRCLE ( 'NONE', #8412, 6.438111078829122036 ) ;
#9357 = VECTOR ( 'NONE', #177, 1000.000000000000000 ) ;
#9358 = CARTESIAN_POINT ( 'NONE',  ( 20.00000000000000000, -5.510910596163090344E-15, 25.00000000000000000 ) ) ;
#9359 = LINE ( 'NONE', #10390, #4033 ) ;
#9360 = EDGE_CURVE ( 'NONE', #7309, #13816, #6985, .T. ) ;
#9361 = VECTOR ( 'NONE', #9899, 1000.000000000000000 ) ;
#9362 = LINE ( 'NONE', #2795, #10319 ) ;
#9363 = EDGE_CURVE ( 'NONE', #8001, #1060, #1661, .T. ) ;
#9364 = CARTESIAN_POINT ( 'NONE',  ( 31.80000000000005045, 6.152361115950385938E-15, -2.445499999999975138 ) ) ;
#9365 = VERTEX_POINT ( 'NONE', #8303 ) ;
#9366 = AXIS2_PLACEMENT_3D ( 'NONE', #8848, #14285, #4487 ) ;
#9367 =( GEOMETRIC_REPRESENTATION_CONTEXT ( 3 ) GLOBAL_UNCERTAINTY_ASSIGNED_CONTEXT ( ( #14225 ) ) GLOBAL_UNIT_ASSIGNED_CONTEXT ( ( #7572, #9851, #4723 ) ) REPRESENTATION_CONTEXT ( 'NONE', 'WORKASPACE' ) );
#9368 = ORIENTED_EDGE ( 'NONE', *, *, #465, .F. ) ;
#9369 = AXIS2_PLACEMENT_3D ( 'NONE', #9073, #1319, #380 ) ;
#9370 = FACE_OUTER_BOUND ( 'NONE', #14070, .T. ) ;
#9371 = DIRECTION ( 'NONE',  ( -1.000000000000000000, 0.000000000000000000, 0.000000000000000000 ) ) ;
#9372 = AXIS2_PLACEMENT_3D ( 'NONE', #9358, #2638, #7149 ) ;
#9373 = EDGE_CURVE ( 'NONE', #3543, #721, #11604, .T. ) ;
#9374 = EDGE_LOOP ( 'NONE', ( #7798, #3498, #398, #14403, #8042 ) ) ;
#9375 =( GEOMETRIC_REPRESENTATION_CONTEXT ( 3 ) GLOBAL_UNCERTAINTY_ASSIGNED_CONTEXT ( ( #13792 ) ) GLOBAL_UNIT_ASSIGNED_CONTEXT ( ( #10331, #3610, #7840 ) ) REPRESENTATION_CONTEXT ( 'NONE', 'WORKASPACE' ) );
#9376 = VECTOR ( 'NONE', #7757, 1000.000000000000000 ) ;
#9377 = EDGE_LOOP ( 'NONE', ( #5445, #13705 ) ) ;
#9378 = DIRECTION ( 'NONE',  ( 0.000000000000000000, 0.000000000000000000, 1.000000000000000000 ) ) ;
#9379 = DIRECTION ( 'NONE',  ( 0.000000000000000000, 0.000000000000000000, 1.000000000000000000 ) ) ;
#9380 = ORIENTED_EDGE ( 'NONE', *, *, #8331, .F. ) ;
#9381 = CARTESIAN_POINT ( 'NONE',  ( -5.253368672218639013, -3.033033817057793957, -4.659491423763650886 ) ) ;
#9382 = ORIENTED_EDGE ( 'NONE', *, *, #11245, .F. ) ;
#9383 = VECTOR ( 'NONE', #3345, 1000.000000000000000 ) ;
#9384 = UNCERTAINTY_MEASURE_WITH_UNIT (LENGTH_MEASURE( 1.000000000000000082E-05 ), #471, 'distance_accuracy_value', 'NONE');
#9385 = AXIS2_PLACEMENT_3D ( 'NONE', #5893, #1444, #8087 ) ;
#9386 = CIRCLE ( 'NONE', #8692, 2.500000000000002220 ) ;
#9387 = CARTESIAN_POINT ( 'NONE',  ( -1.393927851585480271, 4.043713361053534960, -3.226374918436821559 ) ) ;
#9388 = CARTESIAN_POINT ( 'NONE',  ( -3.199999999999999289, -1.586475856045371110E-16, 2.400000000000013234 ) ) ;
#9389 = CARTESIAN_POINT ( 'NONE',  ( 118.6817075744280316, 109.5765550933604828, 0.000000000000000000 ) ) ;
#9390 = FACE_OUTER_BOUND ( 'NONE', #4629, .T. ) ;
#9391 = LINE ( 'NONE', #7263, #5747 ) ;
#9392 = CARTESIAN_POINT ( 'NONE',  ( 13.00000000000000533, 29.99999999999999289, 8.000000000000007105 ) ) ;
#9393 = ADVANCED_FACE ( 'NONE', ( #13897, #1581, #7290 ), #11837, .T. ) ;
#9394 = SURFACE_STYLE_USAGE ( .BOTH. , #8782 ) ;
#9395 = EDGE_CURVE ( 'NONE', #10382, #6124, #11534, .T. ) ;
#9396 = FACE_OUTER_BOUND ( 'NONE', #4912, .T. ) ;
#9397 = VECTOR ( 'NONE', #2011, 1000.000000000000000 ) ;
#9398 = VECTOR ( 'NONE', #5562, 1000.000000000000114 ) ;
#9399 = DIRECTION ( 'NONE',  ( -1.000000000000000000, -1.723842398015259277E-15, 0.000000000000000000 ) ) ;
#9400 = VERTEX_POINT ( 'NONE', #10592 ) ;
#9401 = FACE_OUTER_BOUND ( 'NONE', #5078, .T. ) ;
#9402 = CARTESIAN_POINT ( 'NONE',  ( 4.859329672867496619, 4.267091032106366200, 0.6091815318702697990 ) ) ;
#9403 = CARTESIAN_POINT ( 'NONE',  ( 76.68170757442798902, 124.5765550933606249, -25.00000000000000000 ) ) ;
#9404 = ORIENTED_EDGE ( 'NONE', *, *, #9773, .T. ) ;
#9405 = ORIENTED_EDGE ( 'NONE', *, *, #7205, .F. ) ;
#9406 = ORIENTED_EDGE ( 'NONE', *, *, #6043, .F. ) ;
#9407 = CARTESIAN_POINT ( 'NONE',  ( -5.204170427930318053E-18, 1.332267629550187849E-15, 3.000000000000003553 ) ) ;
#9408 = CARTESIAN_POINT ( 'NONE',  ( 59.10586122665984732, -20.42344490663941414, -35.00000000000000000 ) ) ;
#9409 = ADVANCED_FACE ( 'NONE', ( #9494, #3719, #8160 ), #2614, .T. ) ;
#9410 = COLOUR_RGB ( '', 0.09019608, 0.27058824, 0.51372549) ;
#9411 = ORIENTED_EDGE ( 'NONE', *, *, #1404, .F. ) ;
#9412 = PLANE ( 'NONE',  #1398 ) ;
#9413 = VECTOR ( 'NONE', #5543, 1000.000000000000000 ) ;
#9414 = PRODUCT_DEFINITION_SHAPE ( 'NONE', 'NONE',  #14466 ) ;
#9415 = DIRECTION ( 'NONE',  ( -1.000000000000000000, 0.000000000000000000, 0.000000000000000000 ) ) ;
#9416 = DIRECTION ( 'NONE',  ( 0.000000000000000000, 0.000000000000000000, -1.000000000000000000 ) ) ;
#9417 = CARTESIAN_POINT ( 'NONE',  ( 28.00000000000000355, 29.99999999999999645, -25.00000000000000000 ) ) ;
#9418 = CARTESIAN_POINT ( 'NONE',  ( 0.000000000000000000, 0.000000000000000000, 0.000000000000000000 ) ) ;
#9419 = ADVANCED_FACE ( 'NONE', ( #4016 ), #4877, .T. ) ;
#9420 = CARTESIAN_POINT ( 'NONE',  ( 0.3126073911695614882, -2.020725942163792421, -3.500000000000003109 ) ) ;
#9421 = EDGE_CURVE ( 'NONE', #2316, #687, #650, .T. ) ;
#9422 = CARTESIAN_POINT ( 'NONE',  ( -5.360651806498819664E-15, 3.375361811986497873, -1.153701847711626982 ) ) ;
#9423 = CARTESIAN_POINT ( 'NONE',  ( 88.22284556172391490, -83.66032599071898801, 33.00000000000000000 ) ) ;
#9424 = CARTESIAN_POINT ( 'NONE',  ( -5.594483210025202879E-14, -5.773502691896268857, -0.5999999999999894307 ) ) ;
#9425 = VECTOR ( 'NONE', #2510, 1000.000000000000000 ) ;
#9426 = CIRCLE ( 'NONE', #7322, 9.000000000000001776 ) ;
#9427 = ORIENTED_EDGE ( 'NONE', *, *, #9166, .F. ) ;
#9428 = CARTESIAN_POINT ( 'NONE',  ( 71.80728622811317052, -17.99808865627607801, -28.00000000000000000 ) ) ;
#9429 = VERTEX_POINT ( 'NONE', #5958 ) ;
#9430 = ADVANCED_FACE ( 'NONE', ( #9569 ), #12360, .F. ) ;
#9431 = ORIENTED_EDGE ( 'NONE', *, *, #1170, .F. ) ;
#9432 = CARTESIAN_POINT ( 'NONE',  ( 22.00000000000000355, 30.00000000000000711, -25.00000000000000000 ) ) ;
#9433 = CARTESIAN_POINT ( 'NONE',  ( -3.999999999999996447, -3.469446951953614189E-15, 0.000000000000000000 ) ) ;
#9434 = CARTESIAN_POINT ( 'NONE',  ( 21.68170757442808849, 141.2731697022877313, -35.00000000000000000 ) ) ;
#9435 = PRODUCT_DEFINITION_FORMATION_WITH_SPECIFIED_SOURCE ( 'ANY', '', #12326, .NOT_KNOWN. ) ;
#9436 = CARTESIAN_POINT ( 'NONE',  ( -1.752700365193367750E-15, -5.773502691896300831, -6.000000000000005329 ) ) ;
#9437 = DIRECTION ( 'NONE',  ( -1.000000000000000000, 0.000000000000000000, 0.000000000000000000 ) ) ;
#9438 = CARTESIAN_POINT ( 'NONE',  ( 0.000000000000000000, 0.000000000000000000, 0.000000000000000000 ) ) ;
#9439 = CARTESIAN_POINT ( 'NONE',  ( 0.000000000000000000, 0.000000000000000000, -33.00000000000000000 ) ) ;
#9441 = B_SPLINE_CURVE_WITH_KNOTS ( 'NONE', 3,
 ( #5524, #7861, #13168, #13300, #2179, #3277 ),
 .UNSPECIFIED., .F., .F.,
 ( 4, 2, 4 ),
 ( 0.000000000000000000, 0.002383230369971169656, 0.004766460739942339313 ),
 .UNSPECIFIED. ) ;
#9440 = CARTESIAN_POINT ( 'NONE',  ( 4.211140560182201398, 2.431303136016537358, -3.445885042887453231 ) ) ;
#9442 = CARTESIAN_POINT ( 'NONE',  ( 32.42765351673771335, 110.5971499970933536, 25.00000000000000000 ) ) ;
#9443 = B_SPLINE_CURVE_WITH_KNOTS ( 'NONE', 3,
 ( #6426, #8911, #3377, #11179, #1158, #13468, #10084, #76, #4549, #4266, #3439, #1984, #5335, #9798, #8705, #13734 ),
 .UNSPECIFIED., .F., .F.,
 ( 4, 3, 3, 3, 3, 4 ),
 ( 0.000000000000000000, 3.315506744709606176E-05, 6.608280158699775557E-05, 0.0001026520855291457020, 0.0001376952025664786891, 0.0001398064759190601521 ),
 .UNSPECIFIED. ) ;
#9444 = CIRCLE ( 'NONE', #4323, 0.7999999999999999334 ) ;
#9445 = DIRECTION ( 'NONE',  ( 0.000000000000000000, 1.000000000000000000, -0.000000000000000000 ) ) ;
#9446 = VERTEX_POINT ( 'NONE', #4166 ) ;
#9447 = ADVANCED_FACE ( 'NONE', ( #12053 ), #2024, .T. ) ;
#9448 = ORIENTED_EDGE ( 'NONE', *, *, #213, .F. ) ;
#9449 = CARTESIAN_POINT ( 'NONE',  ( 108.6817075744280174, 29.57655509336062849, -117.0000000000000000 ) ) ;
#9450 = CARTESIAN_POINT ( 'NONE',  ( 22.00000000000000000, 67.00000000000000000, -25.00000000000000000 ) ) ;
#9451 =( BOUNDED_SURFACE ( )  B_SPLINE_SURFACE ( 3, 2, ( 
 ( #3220, #5404, #8627 ),
 ( #5331, #13110, #13183 ),
 ( #3156, #9941, #1082 ),
 ( #3374, #9794, #2262 ),
 ( #3088, #13401, #12214 ),
 ( #14271, #7515, #12003 ) ),
 .UNSPECIFIED., .F., .F., .F. ) 
 B_SPLINE_SURFACE_WITH_KNOTS ( ( 4, 2, 4 ),
 ( 3, 3 ),
 ( 0.02018219363417822834, 0.02264238182714343323, 0.02510257002010863811 ),
 ( 0.000000000000000000, 1.000000000000000000 ),
 .UNSPECIFIED. ) 
 GEOMETRIC_REPRESENTATION_ITEM ( )  RATIONAL_B_SPLINE_SURFACE ( (
 ( 1.000000000000000000, 0.8047781633350724606, 1.000000000000000000),
 ( 1.000000000000000000, 0.8123767859461576979, 1.000000000000000000),
 ( 1.000000000000000000, 0.8190657615682831461, 1.000000000000000000),
 ( 1.000000000000000000, 0.8192365618914937420, 1.000000000000000000),
 ( 1.000000000000000000, 0.8126137554627822501, 1.000000000000000000),
 ( 1.000000000000000000, 0.8047712275319380826, 1.000000000000000000) ) ) 
 REPRESENTATION_ITEM ( '' )  SURFACE ( )  );
#9452 =( NAMED_UNIT ( * ) SI_UNIT ( $, .STERADIAN. ) SOLID_ANGLE_UNIT ( ) );
#9453 = ORIENTED_EDGE ( 'NONE', *, *, #13465, .F. ) ;
#9454 = DIRECTION ( 'NONE',  ( 0.000000000000000000, 0.000000000000000000, -1.000000000000000000 ) ) ;
#9455 = CARTESIAN_POINT ( 'NONE',  ( 5.046772446839294268, 2.317775331972806274, -4.014504635506718877 ) ) ;
#9456 = ORIENTED_EDGE ( 'NONE', *, *, #674, .F. ) ;
#9457 = CLOSED_SHELL ( 'NONE', ( #13774, #1499, #13333, #5937, #13718, #622, #5545, #10743, #11799, #12038, #12713, #5706, #986, #9036, #7599, #3335, #1021, #6905, #9505, #7858, #14159, #14025, #13824, #9913, #5128, #1543, #10620, #8778, #10280, #135, #14353, #14341, #8032, #1271, #1136, #8177, #9965, #10053, #3478 ) ) ;
#9458 = CARTESIAN_POINT ( 'NONE',  ( 33.99999999999998579, 80.00000000000000000, 23.00000000000000000 ) ) ;
#9459 = VERTEX_POINT ( 'NONE', #11910 ) ;
#9460 = EDGE_CURVE ( 'NONE', #6243, #11486, #7198, .T. ) ;
#9461 = EDGE_CURVE ( 'NONE', #375, #6345, #11984, .T. ) ;
#9462 = B_SPLINE_CURVE_WITH_KNOTS ( 'NONE', 3,
 ( #9424, #3873, #583, #8308, #12785, #13425, #12867, #9779 ),
 .UNSPECIFIED., .F., .F.,
 ( 4, 2, 2, 4 ),
 ( 2.451332857528375667E-07, 0.001475502392055722152, 0.002213131021440706107, 0.002950759650825690496 ),
 .UNSPECIFIED. ) ;
#9463 = CARTESIAN_POINT ( 'NONE',  ( 0.000000000000000000, 4.862606272033096033, -3.445885042887453231 ) ) ;
#9464 = CARTESIAN_POINT ( 'NONE',  ( 4.175326769692831341, 2.060699556488946538, 3.569236330973450944 ) ) ;
#9465 = CARTESIAN_POINT ( 'NONE',  ( 21.68170757442806362, 141.2731697022877313, 25.00000000000000000 ) ) ;
#9466 = EDGE_LOOP ( 'NONE', ( #9951, #11293, #12306, #13016, #11211 ) ) ;
#9467 = CARTESIAN_POINT ( 'NONE',  ( 20.00000000000000000, 47.00000000000000000, -25.00000000000000000 ) ) ;
#9468 = CARTESIAN_POINT ( 'NONE',  ( 18.68170757442808849, 141.2731697022877313, 35.00000000000000000 ) ) ;
#9469 =( NAMED_UNIT ( * ) PLANE_ANGLE_UNIT ( ) SI_UNIT ( $, .RADIAN. ) );
#9470 = ORIENTED_EDGE ( 'NONE', *, *, #1040, .F. ) ;
#9471 = DIRECTION ( 'NONE',  ( 2.273843122241288438E-18, 5.551115123125782702E-17, 1.000000000000000000 ) ) ;
#9472 = CARTESIAN_POINT ( 'NONE',  ( 28.00000000000000355, 29.99999999999999645, -25.00000000000000000 ) ) ;
#9473 = EDGE_CURVE ( 'NONE', #9034, #6549, #1066, .T. ) ;
#9474 = ORIENTED_EDGE ( 'NONE', *, *, #2893, .T. ) ;
#9475 = PLANE ( 'NONE',  #954 ) ;
#9476 = ORIENTED_EDGE ( 'NONE', *, *, #8055, .T. ) ;
#9477 = CARTESIAN_POINT ( 'NONE',  ( -129.3408537872145132, 189.5765550933606107, -75.00000000000001421 ) ) ;
#9478 = B_SPLINE_CURVE_WITH_KNOTS ( 'NONE', 3,
 ( #2689, #2763, #1354, #2537 ),
 .UNSPECIFIED., .F., .F.,
 ( 4, 4 ),
 ( 2.380737581434041740E-07, 0.002336974151641588518 ),
 .UNSPECIFIED. ) ;
#9479 = CARTESIAN_POINT ( 'NONE',  ( 4.872112557122744825, -2.415761400130177830E-11, -4.072377784234180176 ) ) ;
#9480 = VERTEX_POINT ( 'NONE', #7716 ) ;
#9481 = CARTESIAN_POINT ( 'NONE',  ( 0.000000000000000000, 40.49999999999999289, 0.000000000000000000 ) ) ;
#9482 = CARTESIAN_POINT ( 'NONE',  ( 4.769962962078715840, 3.046916606660529325, 2.722585630838614712 ) ) ;
#9483 = ORIENTED_EDGE ( 'NONE', *, *, #11788, .F. ) ;
#9484 = CARTESIAN_POINT ( 'NONE',  ( 25.90000000000000213, 29.99999999999999645, 25.00000000000000000 ) ) ;
#9485 = VECTOR ( 'NONE', #4771, 1000.000000000000000 ) ;
#9486 = ORIENTED_EDGE ( 'NONE', *, *, #2194, .T. ) ;
#9487 = ORIENTED_EDGE ( 'NONE', *, *, #1282, .F. ) ;
#9488 = CARTESIAN_POINT ( 'NONE',  ( 20.00000000000000000, -5.510910596163090344E-15, -25.00000000000000000 ) ) ;
#9489 = DIRECTION ( 'NONE',  ( 0.000000000000000000, 0.000000000000000000, 1.000000000000000000 ) ) ;
#9490 = EDGE_LOOP ( 'NONE', ( #3382, #6572, #12651, #3473 ) ) ;
#9491 = CARTESIAN_POINT ( 'NONE',  ( 4.071447262713911996, -4.041451884327377009, 0.000000000000000000 ) ) ;
#9492 = CARTESIAN_POINT ( 'NONE',  ( 76.68170757442798902, 124.5765550933606249, 25.00000000000000000 ) ) ;
#9493 = DIRECTION ( 'NONE',  ( -0.000000000000000000, -1.000000000000000000, -0.000000000000000000 ) ) ;
#9494 = FACE_OUTER_BOUND ( 'NONE', #2478, .T. ) ;
#9495 = SURFACE_STYLE_FILL_AREA ( #10668 ) ;
#9496 = CARTESIAN_POINT ( 'NONE',  ( 58.68170757442803165, 39.57655509336063915, 33.00000000000000000 ) ) ;
#9497 = B_SPLINE_CURVE_WITH_KNOTS ( 'NONE', 3,
 ( #10232, #10309, #1302, #8099 ),
 .UNSPECIFIED., .F., .F.,
 ( 4, 4 ),
 ( 0.000000000000000000, 0.002452478801916362430 ),
 .UNSPECIFIED. ) ;
#9498 = DIRECTION ( 'NONE',  ( 0.2425356250363328581, -0.9701425001453318764, 0.000000000000000000 ) ) ;
#9499 = CARTESIAN_POINT ( 'NONE',  ( 108.6817075744280174, -20.42344490663938572, 33.00000000000002842 ) ) ;
#9500 = FACE_OUTER_BOUND ( 'NONE', #8454, .T. ) ;
#9501 = ORIENTED_EDGE ( 'NONE', *, *, #13563, .T. ) ;
#9502 = ADVANCED_FACE ( 'NONE', ( #8748 ), #1883, .T. ) ;
#9503 = CARTESIAN_POINT ( 'NONE',  ( 4.211140560182201398, 2.431303136016537358, -3.445885042887453231 ) ) ;
#9504 = ORIENTED_EDGE ( 'NONE', *, *, #2982, .F. ) ;
#9505 = ADVANCED_FACE ( 'NONE', ( #3273 ), #891, .T. ) ;
#9506 = VERTEX_POINT ( 'NONE', #12118 ) ;
#9507 = CARTESIAN_POINT ( 'NONE',  ( 36.99999999999999289, 80.00000000000000000, 23.00000000000000000 ) ) ;
#9508 = FACE_OUTER_BOUND ( 'NONE', #12909, .T. ) ;
#9509 = CARTESIAN_POINT ( 'NONE',  ( 59.25585977000769589, 23.28432498401347672, -25.00000000000000000 ) ) ;
#9510 = CARTESIAN_POINT ( 'NONE',  ( -33.49999999999998579, 29.99999999999999645, 8.000000000000007105 ) ) ;
#9511 = CARTESIAN_POINT ( 'NONE',  ( 5.084394237956035845, -2.335963250529156543, -4.046007034530258117 ) ) ;
#9512 = AXIS2_PLACEMENT_3D ( 'NONE', #13936, #3909, #7772 ) ;
#9513 = CARTESIAN_POINT ( 'NONE',  ( -108.6817075744280316, -30.42344490663958112, -32.00000000000002842 ) ) ;
#9514 = CARTESIAN_POINT ( 'NONE',  ( -99.68170757442806007, 69.57655509336049704, -1.796302897001672910E-14 ) ) ;
#9515 = DIRECTION ( 'NONE',  ( 0.000000000000000000, 0.000000000000000000, 1.000000000000000000 ) ) ;
#9516 = FACE_OUTER_BOUND ( 'NONE', #3527, .T. ) ;
#9517 = EDGE_CURVE ( 'NONE', #3097, #13484, #7632, .T. ) ;
#9518 = DIRECTION ( 'NONE',  ( -1.000000000000000000, -3.286707217423839940E-17, -2.273843122241288053E-18 ) ) ;
#9519 = ORIENTED_EDGE ( 'NONE', *, *, #9275, .F. ) ;
#9520 = EDGE_CURVE ( 'NONE', #4078, #13851, #11010, .T. ) ;
#9521 = EDGE_LOOP ( 'NONE', ( #1675, #5709, #12715, #4043 ) ) ;
#9522 = B_SPLINE_CURVE_WITH_KNOTS ( 'NONE', 3,
 ( #9298, #8265, #12515, #9221, #10245, #3675, #1390, #9146 ),
 .UNSPECIFIED., .F., .F.,
 ( 4, 2, 2, 4 ),
 ( 2.465131517103448553E-07, 0.001183067374689843708, 0.001774477805458910071, 0.002365888236227976869 ),
 .UNSPECIFIED. ) ;
#9523 = VERTEX_POINT ( 'NONE', #4103 ) ;
#9524 = DIRECTION ( 'NONE',  ( 0.000000000000000000, 0.000000000000000000, 1.000000000000000000 ) ) ;
#9525 = CYLINDRICAL_SURFACE ( 'NONE', #2333, 8.000000000000000000 ) ;
#9526 = ORIENTED_EDGE ( 'NONE', *, *, #418, .F. ) ;
#9527 = ORIENTED_EDGE ( 'NONE', *, *, #6356, .T. ) ;
#9528 = AXIS2_PLACEMENT_3D ( 'NONE', #2454, #11587, #5790 ) ;
#9529 = DIRECTION ( 'NONE',  ( 0.000000000000000000, 0.4999999999999996669, 0.8660254037844388186 ) ) ;
#9530 = EDGE_CURVE ( 'NONE', #3255, #7437, #14251, .T. ) ;
#9531 = DIRECTION ( 'NONE',  ( -2.273843122241288438E-18, -5.551115123125783935E-17, -1.000000000000000000 ) ) ;
#9532 = ORIENTED_EDGE ( 'NONE', *, *, #5851, .F. ) ;
#9533 = CARTESIAN_POINT ( 'NONE',  ( 1.560000000000005826, -1.732050807568885631, 0.000000000000000000 ) ) ;
#9534 = UNCERTAINTY_MEASURE_WITH_UNIT (LENGTH_MEASURE( 1.000000000000000082E-05 ), #12320, 'distance_accuracy_value', 'NONE');
#9535 = EDGE_CURVE ( 'NONE', #9644, #1073, #8537, .T. ) ;
#9536 = CARTESIAN_POINT ( 'NONE',  ( 2.371692252312040555E-15, 0.3911686820596244063, -4.000000000000003553 ) ) ;
#9537 = DIRECTION ( 'NONE',  ( 1.000000000000000000, 0.000000000000000000, 0.000000000000000000 ) ) ;
#9538 = DIRECTION ( 'NONE',  ( -0.9701425001453318764, -0.2425356250363329969, 0.000000000000000000 ) ) ;
#9539 = CIRCLE ( 'NONE', #7647, 2.750000000000003997 ) ;
#9540 = ORIENTED_EDGE ( 'NONE', *, *, #7252, .T. ) ;
#9541 = VECTOR ( 'NONE', #5030, 1000.000000000000000 ) ;
#9542 = CARTESIAN_POINT ( 'NONE',  ( 2.500000000000000444, 3.469446951953614189E-15, -5.624496230895170257 ) ) ;
#9543 = CARTESIAN_POINT ( 'NONE',  ( 60.00000000000000000, -6.123233995736768255E-16, 25.00000000000000000 ) ) ;
#9544 =( NAMED_UNIT ( * ) PLANE_ANGLE_UNIT ( ) SI_UNIT ( $, .RADIAN. ) );
#9545 = EDGE_LOOP ( 'NONE', ( #8090, #5104, #449, #7304 ) ) ;
#9546 = CARTESIAN_POINT ( 'NONE',  ( 4.400655246570535972, 3.515428273946802129, -4.476900509771682302 ) ) ;
#9547 = AXIS2_PLACEMENT_3D ( 'NONE', #14182, #9848, #13018 ) ;
#9548 = DIRECTION ( 'NONE',  ( 0.000000000000000000, 0.000000000000000000, -1.000000000000000000 ) ) ;
#9549 = EDGE_LOOP ( 'NONE', ( #9246, #13391, #6452, #13924 ) ) ;
#9550 = CYLINDRICAL_SURFACE ( 'NONE', #4927, 9.000000000000001776 ) ;
#9551 = CARTESIAN_POINT ( 'NONE',  ( 6.800000000000028244, -4.618802153517003184, 0.000000000000000000 ) ) ;
#9552 = ADVANCED_FACE ( 'NONE', ( #5247 ), #1982, .F. ) ;
#9553 = PRODUCT_RELATED_PRODUCT_CATEGORY ( 'part', '', ( #12672 ) ) ;
#9554 = LINE ( 'NONE', #14237, #9397 ) ;
#9555 = ORIENTED_EDGE ( 'NONE', *, *, #7318, .F. ) ;
#9556 = PLANE ( 'NONE',  #656 ) ;
#9557 = CARTESIAN_POINT ( 'NONE',  ( 4.847001880571993659, 3.049720480807994516, 2.717729178357345177 ) ) ;
#9558 = AXIS2_PLACEMENT_3D ( 'NONE', #14184, #14046, #4102 ) ;
#9559 = DIRECTION ( 'NONE',  ( 0.000000000000000000, 0.000000000000000000, -1.000000000000000000 ) ) ;
#9560 = EDGE_LOOP ( 'NONE', ( #13702, #292, #9065, #14057, #14058 ) ) ;
#9561 = VERTEX_POINT ( 'NONE', #12267 ) ;
#9562 = CARTESIAN_POINT ( 'NONE',  ( 21.68170757442808849, 141.2731697022877313, -25.00000000000000000 ) ) ;
#9563 = CARTESIAN_POINT ( 'NONE',  ( -3.868554393999076968, 47.50270580730570202, 5.050781263000355459 ) ) ;
#9564 = VERTEX_POINT ( 'NONE', #11366 ) ;
#9565 = CARTESIAN_POINT ( 'NONE',  ( 4.033901012035909339, 3.740908793662586884, -0.5205559028927313481 ) ) ;
#9566 = LINE ( 'NONE', #7361, #7868 ) ;
#9567 = ORIENTED_EDGE ( 'NONE', *, *, #11848, .T. ) ;
#9568 = DIRECTION ( 'NONE',  ( -0.9701425001453319874, -0.2425356250363328858, 0.000000000000000000 ) ) ;
#9569 = FACE_OUTER_BOUND ( 'NONE', #10523, .T. ) ;
#9570 = VECTOR ( 'NONE', #635, 1000.000000000000000 ) ;
#9571 = ORIENTED_EDGE ( 'NONE', *, *, #9684, .F. ) ;
#9572 = DIRECTION ( 'NONE',  ( 1.000000000000000000, 3.286707217423839940E-17, 2.273843122241288053E-18 ) ) ;
#9573 = VECTOR ( 'NONE', #800, 1000.000000000000000 ) ;
#9574 = LINE ( 'NONE', #1887, #890 ) ;
#9575 = EDGE_LOOP ( 'NONE', ( #14117, #10643, #8224, #2131 ) ) ;
#9576 = VECTOR ( 'NONE', #5399, 1000.000000000000000 ) ;
#9577 = LINE ( 'NONE', #10602, #12960 ) ;
#9578 = ORIENTED_EDGE ( 'NONE', *, *, #2222, .F. ) ;
#9579 = EDGE_LOOP ( 'NONE', ( #14146, #1003, #12891 ) ) ;
#9580 = DIRECTION ( 'NONE',  ( 0.2425356250363304988, -0.9701425001453325425, -0.000000000000000000 ) ) ;
#9581 = LINE ( 'NONE', #1680, #4672 ) ;
#9582 = CARTESIAN_POINT ( 'NONE',  ( 0.000000000000000000, 19.49999999999999645, 8.000000000000007105 ) ) ;
#9583 = CARTESIAN_POINT ( 'NONE',  ( 20.00000000000000000, 70.00000000000000000, 25.00000000000000000 ) ) ;
#9584 = DIRECTION ( 'NONE',  ( -1.000000000000000000, 0.000000000000000000, 0.000000000000000000 ) ) ;
#9585 = SHAPE_DEFINITION_REPRESENTATION ( #5999, #7389 ) ;
#9586 = CARTESIAN_POINT ( 'NONE',  ( -5.551115123125782702E-14, -3.464101615137743728, -2.000000000000015543 ) ) ;
#9587 = DIRECTION ( 'NONE',  ( 0.000000000000000000, 0.000000000000000000, 1.000000000000000000 ) ) ;
#9588 = VECTOR ( 'NONE', #4753, 1000.000000000000000 ) ;
#9589 = ADVANCED_FACE ( 'NONE', ( #2518 ), #13290, .T. ) ;
#9590 = ORIENTED_EDGE ( 'NONE', *, *, #4165, .T. ) ;
#9591 = CARTESIAN_POINT ( 'NONE',  ( -129.3408537872145132, 189.5765550933606107, -9.000000000000007105 ) ) ;
#9592 = ORIENTED_EDGE ( 'NONE', *, *, #14087, .F. ) ;
#9593 = AXIS2_PLACEMENT_3D ( 'NONE', #2465, #6914, #6029 ) ;
#9594 = CARTESIAN_POINT ( 'NONE',  ( -8.000000000000000000, 25.49999999999996803, 8.000000000000007105 ) ) ;
#9595 = DIRECTION ( 'NONE',  ( -1.000000000000000000, 1.224646799147352714E-16, 0.000000000000000000 ) ) ;
#9596 = EDGE_CURVE ( 'NONE', #8261, #12769, #11013, .T. ) ;
#9597 = EDGE_LOOP ( 'NONE', ( #1280, #1972 ) ) ;
#9598 = EDGE_CURVE ( 'NONE', #6152, #3422, #10135, .T. ) ;
#9599 = DIRECTION ( 'NONE',  ( 1.000000000000000000, 0.000000000000000000, 0.000000000000000000 ) ) ;
#9600 = CIRCLE ( 'NONE', #11463, 13.00000000000002487 ) ;
#9601 = PRESENTATION_LAYER_ASSIGNMENT (  '', '', ( #8435 ) ) ;
#9602 = CARTESIAN_POINT ( 'NONE',  ( -118.6817075744283727, 189.5765550933606107, -117.0000000000000000 ) ) ;
#9603 = ORIENTED_EDGE ( 'NONE', *, *, #6981, .F. ) ;
#9604 = LINE ( 'NONE', #8425, #5904 ) ;
#9605 = CARTESIAN_POINT ( 'NONE',  ( -5.253368672218636348, 3.033033817057773085, -4.659491423763650886 ) ) ;
#9606 = CARTESIAN_POINT ( 'NONE',  ( 0.000000000000000000, -3.031088913245549854, -1.750000000000001554 ) ) ;
#9607 = CARTESIAN_POINT ( 'NONE',  ( -31.44014396567295577, 38.31657438465165200, 0.000000000000000000 ) ) ;
#9608 = ORIENTED_EDGE ( 'NONE', *, *, #3975, .T. ) ;
#9609 = EDGE_CURVE ( 'NONE', #13816, #2841, #3005, .T. ) ;
#9610 = VECTOR ( 'NONE', #12646, 1000.000000000000000 ) ;
#9611 = DIRECTION ( 'NONE',  ( 0.000000000000000000, 0.000000000000000000, 1.000000000000000000 ) ) ;
#9612 = VECTOR ( 'NONE', #4826, 1000.000000000000000 ) ;
#9613 = CARTESIAN_POINT ( 'NONE',  ( 53.99999999999997868, -1.324077043022348342E-15, 23.00000000000000000 ) ) ;
#9614 = ORIENTED_EDGE ( 'NONE', *, *, #4501, .F. ) ;
#9615 = EDGE_LOOP ( 'NONE', ( #8684, #12110 ) ) ;
#9616 = CARTESIAN_POINT ( 'NONE',  ( 28.00000000000000355, 29.99999999999999645, 6.999999999999992006 ) ) ;
#9617 = ORIENTED_EDGE ( 'NONE', *, *, #13491, .F. ) ;
#9618 = PRESENTATION_STYLE_ASSIGNMENT (( #9394 ) ) ;
#9619 = PLANE ( 'NONE',  #2757 ) ;
#9620 = CARTESIAN_POINT ( 'NONE',  ( 76.68170757442801744, 144.5765550933605823, 33.00000000000000000 ) ) ;
#9621 = ORIENTED_EDGE ( 'NONE', *, *, #4600, .F. ) ;
#9622 = LINE ( 'NONE', #14107, #8581 ) ;
#9623 = VECTOR ( 'NONE', #8401, 1000.000000000000000 ) ;
#9624 = FACE_OUTER_BOUND ( 'NONE', #8151, .T. ) ;
#9625 = AXIS2_PLACEMENT_3D ( 'NONE', #5555, #11124, #8923 ) ;
#9626 = ORIENTED_EDGE ( 'NONE', *, *, #4591, .T. ) ;
#9627 = ORIENTED_EDGE ( 'NONE', *, *, #312, .T. ) ;
#9628 = CARTESIAN_POINT ( 'NONE',  ( -3.861362476283257905, -2.629030857716000646, -3.371615880910393326 ) ) ;
#9629 = LINE ( 'NONE', #907, #14311 ) ;
#9630 = EDGE_CURVE ( 'NONE', #8264, #5579, #13654, .T. ) ;
#9631 = ORIENTED_EDGE ( 'NONE', *, *, #3611, .F. ) ;
#9632 = CARTESIAN_POINT ( 'NONE',  ( 5.103021810857296892, -2.353405741490973035, 4.076218315086694410 ) ) ;
#9633 = DIRECTION ( 'NONE',  ( 0.000000000000000000, 0.4999999999999997780, -0.8660254037844387076 ) ) ;
#9634 = AXIS2_PLACEMENT_3D ( 'NONE', #9408, #13676, #9181 ) ;
#9635 = CARTESIAN_POINT ( 'NONE',  ( 53.99999999999997868, -1.324077043022348342E-15, 23.00000000000000000 ) ) ;
#9636 = DIRECTION ( 'NONE',  ( 0.000000000000000000, 0.000000000000000000, 1.000000000000000000 ) ) ;
#9637 = CIRCLE ( 'NONE', #11039, 2.499999999999999112 ) ;
#9638 = ORIENTED_EDGE ( 'NONE', *, *, #9275, .T. ) ;
#9639 = SURFACE_STYLE_USAGE ( .BOTH. , #11839 ) ;
#9640 = DIRECTION ( 'NONE',  ( 0.000000000000000000, 0.000000000000000000, 1.000000000000000000 ) ) ;
#9641 = DIRECTION ( 'NONE',  ( 0.000000000000000000, -0.000000000000000000, 1.000000000000000000 ) ) ;
#9642 = ORIENTED_EDGE ( 'NONE', *, *, #6099, .T. ) ;
#9643 = MECHANICAL_DESIGN_GEOMETRIC_PRESENTATION_REPRESENTATION (  '', ( #3820 ), #6369 ) ;
#9644 = VERTEX_POINT ( 'NONE', #6689 ) ;
#9645 = AXIS2_PLACEMENT_3D ( 'NONE', #10796, #7479, #5235 ) ;
#9646 = VECTOR ( 'NONE', #4754, 1000.000000000000000 ) ;
#9647 = ORIENTED_EDGE ( 'NONE', *, *, #6363, .F. ) ;
#9648 = DIRECTION ( 'NONE',  ( 0.000000000000000000, 1.000000000000000000, 0.000000000000000000 ) ) ;
#9649 = ORIENTED_EDGE ( 'NONE', *, *, #7208, .T. ) ;
#9650 = EDGE_CURVE ( 'NONE', #13002, #7536, #6733, .T. ) ;
#9651 = EDGE_LOOP ( 'NONE', ( #7407, #8275, #10804, #4752 ) ) ;
#9652 = CARTESIAN_POINT ( 'NONE',  ( 22.00000000000000355, 40.00000000000000711, -25.00000000000000000 ) ) ;
#9653 = EDGE_CURVE ( 'NONE', #3255, #1772, #1340, .T. ) ;
#9654 = LINE ( 'NONE', #10607, #8396 ) ;
#9655 = CARTESIAN_POINT ( 'NONE',  ( 3.790690275325682812, 47.54583148236281431, 2.696316195168958263 ) ) ;
#9656 = LINE ( 'NONE', #9583, #10077 ) ;
#9657 = CARTESIAN_POINT ( 'NONE',  ( 0.000000000000000000, 4.618802153517016507, -3.133295621305376422 ) ) ;
#9658 = PRODUCT_CONTEXT ( 'NONE', #4388, 'mechanical' ) ;
#9659 = DIRECTION ( 'NONE',  ( 0.000000000000000000, 1.000000000000000000, 0.000000000000000000 ) ) ;
#9660 = CARTESIAN_POINT ( 'NONE',  ( 61.60657227073433262, 3.881474981106830313, -25.00000000000000000 ) ) ;
#9661 = AXIS2_PLACEMENT_3D ( 'NONE', #5161, #14108, #11356 ) ;
#9662 = VERTEX_POINT ( 'NONE', #1278 ) ;
#9663 = CARTESIAN_POINT ( 'NONE',  ( 3.057313426867670714, 4.281874658697562452, -4.357628883416062138 ) ) ;
#9664 = EDGE_LOOP ( 'NONE', ( #4653, #1799, #2012 ) ) ;
#9665 = B_SPLINE_CURVE_WITH_KNOTS ( 'NONE', 3,
 ( #11335, #10167, #13550, #85, #6799, #9131, #151, #7894 ),
 .UNSPECIFIED., .F., .F.,
 ( 4, 2, 2, 4 ),
 ( 2.465131517153036509E-07, 0.001183067374689848045, 0.001774477805458914408, 0.002365888236227980772 ),
 .UNSPECIFIED. ) ;
#9666 = ORIENTED_EDGE ( 'NONE', *, *, #5248, .T. ) ;
#9667 = VECTOR ( 'NONE', #9744, 1000.000000000000000 ) ;
#9668 = EDGE_CURVE ( 'NONE', #4104, #10936, #5587, .T. ) ;
#9669 = LINE ( 'NONE', #9449, #13634 ) ;
#9670 = DIRECTION ( 'NONE',  ( 1.000000000000000000, 0.000000000000000000, 0.000000000000000000 ) ) ;
#9672 = VECTOR ( 'NONE', #8312, 1000.000000000000000 ) ;
#9671 = SURFACE_STYLE_USAGE ( .BOTH. , #4278 ) ;
#9673 = VERTEX_POINT ( 'NONE', #7857 ) ;
#9674 = PRODUCT_DEFINITION_FORMATION_WITH_SPECIFIED_SOURCE ( 'ANY', '', #2643, .NOT_KNOWN. ) ;
#9675 = DIRECTION ( 'NONE',  ( 0.000000000000000000, 0.000000000000000000, -1.000000000000000000 ) ) ;
#9676 = CARTESIAN_POINT ( 'NONE',  ( 4.000000000000003553, 2.309401076758511806, -0.5000000000000004441 ) ) ;
#9677 = EDGE_LOOP ( 'NONE', ( #11795, #12408, #8641, #9592 ) ) ;
#9678 = EDGE_CURVE ( 'NONE', #3061, #9023, #2307, .T. ) ;
#9679 = CARTESIAN_POINT ( 'NONE',  ( 4.071447262713911996, 2.020725942163681399, -3.499999999999996003 ) ) ;
#9680 = ORIENTED_EDGE ( 'NONE', *, *, #10352, .F. ) ;
#9681 = VECTOR ( 'NONE', #3059, 1000.000000000000000 ) ;
#9682 = ORIENTED_EDGE ( 'NONE', *, *, #5138, .F. ) ;
#9683 = UNCERTAINTY_MEASURE_WITH_UNIT (LENGTH_MEASURE( 1.000000000000000082E-05 ), #4317, 'distance_accuracy_value', 'NONE');
#9684 = EDGE_CURVE ( 'NONE', #3625, #13865, #252, .T. ) ;
#9685 = CARTESIAN_POINT ( 'NONE',  ( -5.029394918168159201, 2.903722509865322543, -4.451004066889655775 ) ) ;
#9686 = CARTESIAN_POINT ( 'NONE',  ( 5.248984340851196251, 2.531668808681887928, -4.566868479993924090 ) ) ;
#9687 = DIRECTION ( 'NONE',  ( -1.000000000000000000, -3.286707217423839940E-17, 2.273843122241290364E-18 ) ) ;
#9688 = EDGE_CURVE ( 'NONE', #13851, #13075, #8355, .T. ) ;
#9689 = ORIENTED_EDGE ( 'NONE', *, *, #7917, .F. ) ;
#9690 = CARTESIAN_POINT ( 'NONE',  ( 4.175572532730952524, 4.122058607836114774, -1.739027647669125673E-15 ) ) ;
#9691 = CARTESIAN_POINT ( 'NONE',  ( 5.108705755340869459, -2.382235250128048154, -4.077515506918746979 ) ) ;
#9692 = ORIENTED_EDGE ( 'NONE', *, *, #9327, .F. ) ;
#9693 = CARTESIAN_POINT ( 'NONE',  ( -13.00000000000000533, 24.50000000000001421, 8.000000000000007105 ) ) ;
#9694 = ORIENTED_EDGE ( 'NONE', *, *, #2805, .T. ) ;
#9695 = DIRECTION ( 'NONE',  ( 0.000000000000000000, -1.000000000000000000, 0.000000000000000000 ) ) ;
#9696 = VECTOR ( 'NONE', #4816, 1000.000000000000000 ) ;
#9697 = CARTESIAN_POINT ( 'NONE',  ( -118.6817075744282306, 109.5765550933602697, 0.000000000000000000 ) ) ;
#9698 = CARTESIAN_POINT ( 'NONE',  ( 40.00000000000000711, 80.00000000000000000, -25.00000000000000000 ) ) ;
#9699 = ORIENTED_EDGE ( 'NONE', *, *, #3601, .F. ) ;
#9700 = FACE_OUTER_BOUND ( 'NONE', #14369, .T. ) ;
#9701 = ADVANCED_FACE ( 'NONE', ( #9020 ), #8958, .F. ) ;
#9702 = CARTESIAN_POINT ( 'NONE',  ( 5.000000000000000000, -2.886751345948148639, -4.284345921091780696 ) ) ;
#9703 = ORIENTED_EDGE ( 'NONE', *, *, #3251, .T. ) ;
#9704 = CARTESIAN_POINT ( 'NONE',  ( -2.750000000000003553, 40.49999999999999289, 8.000000000000007105 ) ) ;
#9705 = CARTESIAN_POINT ( 'NONE',  ( -2.448955312130046469, 48.11928591936100474, 0.8265499080465856796 ) ) ;
#9706 = B_SPLINE_CURVE_WITH_KNOTS ( 'NONE', 3,
 ( #8278, #392, #13794, #12676, #5782, #7176, #12596, #1406, #7034, #3624, #9162, #3760, #2443, #9464, #9237, #11508 ),
 .UNSPECIFIED., .F., .F.,
 ( 4, 3, 3, 3, 3, 4 ),
 ( 0.000000000000000000, 3.315506744709051878E-05, 6.608280158698574803E-05, 0.0001026520855291322985, 0.0001376952025664795836, 0.0001398064759190602334 ),
 .UNSPECIFIED. ) ;
#9707 = ORIENTED_EDGE ( 'NONE', *, *, #12835, .T. ) ;
#9708 = DIRECTION ( 'NONE',  ( 0.000000000000000000, -8.482162385747133845E-47, 1.000000000000000000 ) ) ;
#9709 = PLANE ( 'NONE',  #3026 ) ;
#9710 = DIRECTION ( 'NONE',  ( 0.000000000000000000, 1.000000000000000000, 0.000000000000000000 ) ) ;
#9711 = ORIENTED_EDGE ( 'NONE', *, *, #7703, .T. ) ;
#9712 = DIRECTION ( 'NONE',  ( 0.000000000000000000, 4.440892098500621231E-16, 1.000000000000000000 ) ) ;
#9713 = CARTESIAN_POINT ( 'NONE',  ( 24.99999999999999289, -4.898587196589414604E-15, 25.00000000000000000 ) ) ;
#9714 = CARTESIAN_POINT ( 'NONE',  ( 0.000000000000000000, 189.5765550933606107, -37.00000000000003553 ) ) ;
#9715 = EDGE_CURVE ( 'NONE', #10016, #4769, #6265, .T. ) ;
#9716 = ORIENTED_EDGE ( 'NONE', *, *, #1546, .F. ) ;
#9717 = ORIENTED_EDGE ( 'NONE', *, *, #125, .F. ) ;
#9718 = CARTESIAN_POINT ( 'NONE',  ( 60.00000000000000000, -6.123233995736768255E-16, -25.00000000000000000 ) ) ;
#9719 = ORIENTED_EDGE ( 'NONE', *, *, #9807, .T. ) ;
#9720 = EDGE_LOOP ( 'NONE', ( #2810, #6882 ) ) ;
#9721 = DIRECTION ( 'NONE',  ( -1.000000000000000000, -2.312964634635743450E-16, 0.000000000000000000 ) ) ;
#9722 = CYLINDRICAL_SURFACE ( 'NONE', #7223, 2.500000000000002220 ) ;
#9723 = CARTESIAN_POINT ( 'NONE',  ( 3.012791009409891085, 47.91354231080892134, 6.643648411893779304 ) ) ;
#9724 = FACE_OUTER_BOUND ( 'NONE', #9999, .T. ) ;
#9725 = CARTESIAN_POINT ( 'NONE',  ( 76.68170757442796059, 3.003422806631532356E-13, 33.00000000000000000 ) ) ;
#9726 = APPLICATION_PROTOCOL_DEFINITION ( 'draft international standard', 'automotive_design', 1998, #11289 ) ;
#9727 = CARTESIAN_POINT ( 'NONE',  ( 2.750000000000002665, 0.000000000000000000, 0.000000000000000000 ) ) ;
#9728 = CARTESIAN_POINT ( 'NONE',  ( 31.44014396567294867, 21.68342561534834090, 0.000000000000000000 ) ) ;
#9729 = ORIENTED_EDGE ( 'NONE', *, *, #4246, .T. ) ;
#9730 = ADVANCED_FACE ( 'NONE', ( #8285 ), #3851, .F. ) ;
#9731 = PRODUCT_DEFINITION ( 'UNKNOWN', '', #2915, #14371 ) ;
#9732 = ADVANCED_FACE ( 'NONE', ( #9317 ), #12681, .F. ) ;
#9733 = DIRECTION ( 'NONE',  ( -0.000000000000000000, 1.000000000000000000, -0.000000000000000000 ) ) ;
#9734 = ORIENTED_EDGE ( 'NONE', *, *, #12499, .F. ) ;
#9735 = ORIENTED_EDGE ( 'NONE', *, *, #756, .F. ) ;
#9736 = VECTOR ( 'NONE', #8512, 1000.000000000000000 ) ;
#9737 = DIRECTION ( 'NONE',  ( 1.000000000000000000, 0.000000000000000000, 0.000000000000000000 ) ) ;
#9738 = LINE ( 'NONE', #5749, #11924 ) ;
#9739 = CARTESIAN_POINT ( 'NONE',  ( 5.551115123125782702E-14, 3.464101615137764156, 2.000000000000001776 ) ) ;
#9740 = VERTEX_POINT ( 'NONE', #7186 ) ;
#9741 = CARTESIAN_POINT ( 'NONE',  ( 31.38313257588138683, 143.6985259526510390, 28.00000000000000000 ) ) ;
#9742 = CARTESIAN_POINT ( 'NONE',  ( 5.384454397937120440, 8.966917871450958727E-16, -4.699999999999981526 ) ) ;
#9743 = VECTOR ( 'NONE', #5416, 1000.000000000000114 ) ;
#9744 = DIRECTION ( 'NONE',  ( -0.000000000000000000, 1.000000000000000000, -0.000000000000000000 ) ) ;
#9745 = CONICAL_SURFACE ( 'NONE', #5756, 5.000000000000000888, 0.9110539511682884672 ) ;
#9746 = CARTESIAN_POINT ( 'NONE',  ( 4.000000000000005329, 1.539600717839000099, -3.000726591567076440 ) ) ;
#9747 = DIRECTION ( 'NONE',  ( -1.000000000000000000, 0.000000000000000000, 0.000000000000000000 ) ) ;
#9748 = CARTESIAN_POINT ( 'NONE',  ( 0.3572655899081733644, -2.309401076758484272, 4.000000000000031086 ) ) ;
#9749 = CARTESIAN_POINT ( 'NONE',  ( -5.000000000000001776, -2.886751345948141534, -6.000000000000005329 ) ) ;
#9750 = CARTESIAN_POINT ( 'NONE',  ( 4.966160964381386655, 1.610279710338473391, -4.074842399450050223 ) ) ;
#9751 =( NAMED_UNIT ( * ) PLANE_ANGLE_UNIT ( ) SI_UNIT ( $, .RADIAN. ) );
#9752 = DIRECTION ( 'NONE',  ( 0.000000000000000000, 0.000000000000000000, -1.000000000000000000 ) ) ;
#9753 = TOROIDAL_SURFACE ( 'NONE', #4619, 6.532899837730830939, 0.5671001622691684840 ) ;
#9754 = ORIENTED_EDGE ( 'NONE', *, *, #5541, .F. ) ;
#9755 = ORIENTED_EDGE ( 'NONE', *, *, #13227, .F. ) ;
#9756 = CARTESIAN_POINT ( 'NONE',  ( 4.197393957002307552, 7.823395958202418729E-14, -3.203767560748914445 ) ) ;
#9757 = DIRECTION ( 'NONE',  ( 1.000000000000000000, 0.000000000000000000, 0.000000000000000000 ) ) ;
#9758 = EDGE_CURVE ( 'NONE', #6876, #10272, #3915, .T. ) ;
#9759 = EDGE_LOOP ( 'NONE', ( #12502, #4030, #1609, #1735 ) ) ;
#9760 = DIRECTION ( 'NONE',  ( -1.000000000000000000, -3.286707217423839940E-17, -2.273843122241288053E-18 ) ) ;
#9761 = DIRECTION ( 'NONE',  ( -0.000000000000000000, -0.000000000000000000, -1.000000000000000000 ) ) ;
#9762 = AXIS2_PLACEMENT_3D ( 'NONE', #9741, #11060, #4204 ) ;
#9763 = ORIENTED_EDGE ( 'NONE', *, *, #9005, .F. ) ;
#9764 = CONICAL_SURFACE ( 'NONE', #8342, 5.371010071662830399, 1.221730476396037268 ) ;
#9765 = ORIENTED_EDGE ( 'NONE', *, *, #10470, .F. ) ;
#9766 = DIRECTION ( 'NONE',  ( 0.3420201433256625512, 1.784837759418569071E-16, 0.9396926207859105373 ) ) ;
#9767 = CARTESIAN_POINT ( 'NONE',  ( -1.305984381679703654, 48.39647413643795915, 0.2102513847387771917 ) ) ;
#9768 = ORIENTED_EDGE ( 'NONE', *, *, #4971, .T. ) ;
#9769 = CARTESIAN_POINT ( 'NONE',  ( 5.103531824934115946, -2.354098498486438373, 4.077418205400141105 ) ) ;
#9770 = CARTESIAN_POINT ( 'NONE',  ( -3.999999999999996447, 2.309401076758494487, -0.5000000000000004441 ) ) ;
#9771 = FACE_OUTER_BOUND ( 'NONE', #13174, .T. ) ;
#9772 = VERTEX_POINT ( 'NONE', #11662 ) ;
#9773 = EDGE_CURVE ( 'NONE', #11937, #5807, #10932, .T. ) ;
#9774 = CARTESIAN_POINT ( 'NONE',  ( 4.052432342741418836, 1.393590342654194680, 3.567979436357489043 ) ) ;
#9775 = AXIS2_PLACEMENT_3D ( 'NONE', #12056, #719, #9641 ) ;
#9776 = PLANE ( 'NONE',  #5549 ) ;
#9777 = AXIS2_PLACEMENT_3D ( 'NONE', #2746, #1560, #3766 ) ;
#9778 = EDGE_CURVE ( 'NONE', #3003, #11268, #7651, .T. ) ;
#9779 = CARTESIAN_POINT ( 'NONE',  ( -2.500000000000016875, -4.330127018922186544, 0.000000000000000000 ) ) ;
#9780 = VECTOR ( 'NONE', #7996, 1000.000000000000000 ) ;
#9781 = B_SPLINE_CURVE_WITH_KNOTS ( 'NONE', 3,
 ( #11576, #10485, #467, #4922, #9387, #13870, #5004, #9463 ),
 .UNSPECIFIED., .F., .F.,
 ( 4, 2, 2, 4 ),
 ( 0.000000000000000000, 0.002450665683189815792, 0.003675998524784723689, 0.004901331366379631585 ),
 .UNSPECIFIED. ) ;
#9782 = ORIENTED_EDGE ( 'NONE', *, *, #4236, .F. ) ;
#9783 = EDGE_LOOP ( 'NONE', ( #11812, #1869, #11595, #5365, #1526 ) ) ;
#9784 = CARTESIAN_POINT ( 'NONE',  ( 3.352586340487478278, 3.837886065734358532, -0.05822226285683582137 ) ) ;
#9785 = ORIENTED_EDGE ( 'NONE', *, *, #834, .T. ) ;
#9786 = PRESENTATION_LAYER_ASSIGNMENT (  '', '', ( #10015 ) ) ;
#9787 = CARTESIAN_POINT ( 'NONE',  ( 33.99999999999998579, 80.00000000000000000, 25.00000000000000000 ) ) ;
#9788 = LINE ( 'NONE', #4395, #7679 ) ;
#9789 = CARTESIAN_POINT ( 'NONE',  ( 1.050836307075463827, 48.43494986415684167, 7.868526909826528914 ) ) ;
#9790 = EDGE_CURVE ( 'NONE', #6157, #7901, #10491, .T. ) ;
#9791 = DIRECTION ( 'NONE',  ( -1.000000000000000000, 0.000000000000000000, 0.000000000000000000 ) ) ;
#9792 = DIRECTION ( 'NONE',  ( -0.8571673007021134438, 0.000000000000000000, 0.5150380749100522682 ) ) ;
#9793 = PRODUCT_CONTEXT ( 'NONE', #3629, 'mechanical' ) ;
#9794 = CARTESIAN_POINT ( 'NONE',  ( 3.999999999999998224, 0.8228621380349545600, -3.130611579770202546 ) ) ;
#9795 = APPLICATION_CONTEXT ( 'automotive_design' ) ;
#9796 = CARTESIAN_POINT ( 'NONE',  ( -129.3408537872145132, 199.5765550933606107, -9.000000000000007105 ) ) ;
#9797 = VERTEX_POINT ( 'NONE', #6009 ) ;
#9798 = CARTESIAN_POINT ( 'NONE',  ( 4.175326769692832229, -2.060699556488909678, 3.569236330973486915 ) ) ;
#9799 = AXIS2_PLACEMENT_3D ( 'NONE', #6419, #7511, #9871 ) ;
#9800 = CONICAL_SURFACE ( 'NONE', #13560, 5.000000000000000888, 0.9110539511682884672 ) ;
#9801 = FACE_OUTER_BOUND ( 'NONE', #529, .T. ) ;
#9802 = ORIENTED_EDGE ( 'NONE', *, *, #7103, .T. ) ;
#9803 = CARTESIAN_POINT ( 'NONE',  ( 62.10586122665984732, -20.42344490663941414, 23.00000000000000000 ) ) ;
#9804 = CARTESIAN_POINT ( 'NONE',  ( 0.02993401039713160586, 2.688325911136451030, -2.343682934607757229 ) ) ;
#9805 = EDGE_CURVE ( 'NONE', #9041, #11047, #12810, .T. ) ;
#9806 = DIRECTION ( 'NONE',  ( 1.000000000000000000, 0.000000000000000000, 0.000000000000000000 ) ) ;
#9807 = EDGE_CURVE ( 'NONE', #3835, #6304, #244, .T. ) ;
#9808 = PLANE ( 'NONE',  #7624 ) ;
#9809 = AXIS2_PLACEMENT_3D ( 'NONE', #14376, #9351, #437 ) ;
#9810 = PRESENTATION_STYLE_ASSIGNMENT (( #9671 ) ) ;
#9811 = ORIENTED_EDGE ( 'NONE', *, *, #1743, .F. ) ;
#9812 = DIRECTION ( 'NONE',  ( -1.000000000000000000, 0.000000000000000000, 0.000000000000000000 ) ) ;
#9813 = LINE ( 'NONE', #6510, #8704 ) ;
#9814 = CARTESIAN_POINT ( 'NONE',  ( 20.00000000000000711, 20.00000000000000355, -25.00000000000000000 ) ) ;
#9815 = ORIENTED_EDGE ( 'NONE', *, *, #14294, .T. ) ;
#9816 = AXIS2_PLACEMENT_3D ( 'NONE', #414, #4875, #13605 ) ;
#9817 = CARTESIAN_POINT ( 'NONE',  ( -0.6810530063607231899, -4.461079733297850680, -3.298443181296113025 ) ) ;
#9818 = DIRECTION ( 'NONE',  ( 0.000000000000000000, 0.000000000000000000, 1.000000000000000000 ) ) ;
#9819 = DIRECTION ( 'NONE',  ( -1.000000000000000000, 0.000000000000000000, 0.000000000000000000 ) ) ;
#9820 = CARTESIAN_POINT ( 'NONE',  ( 78.52142056027061301, -86.08568224108226730, -32.99999999999999289 ) ) ;
#9821 = FACE_OUTER_BOUND ( 'NONE', #10619, .T. ) ;
#9822 = CARTESIAN_POINT ( 'NONE',  ( 2.749999999999997780, 25.49999999999996803, 0.000000000000000000 ) ) ;
#9823 = ADVANCED_FACE ( 'NONE', ( #553 ), #5013, .F. ) ;
#9824 = FACE_OUTER_BOUND ( 'NONE', #13372, .T. ) ;
#9825 = EDGE_LOOP ( 'NONE', ( #3413, #4051, #60, #7392 ) ) ;
#9826 = CIRCLE ( 'NONE', #5153, 5.499999999999980460 ) ;
#9827 = CIRCLE ( 'NONE', #5388, 3.499999999999999112 ) ;
#9828 = CARTESIAN_POINT ( 'NONE',  ( 108.6817075744280174, -20.42344490663938572, 33.00000000000002842 ) ) ;
#9829 = AXIS2_PLACEMENT_3D ( 'NONE', #2758, #12613, #7123 ) ;
#9830 = DIRECTION ( 'NONE',  ( -1.000000000000000000, -3.286707217423839940E-17, -2.273843122241288053E-18 ) ) ;
#9831 = VERTEX_POINT ( 'NONE', #2825 ) ;
#9832 = CARTESIAN_POINT ( 'NONE',  ( 33.99999999999998579, 80.00000000000000000, 25.00000000000000000 ) ) ;
#9833 = AXIS2_PLACEMENT_3D ( 'NONE', #4968, #2092, #6129 ) ;
#9834 = FACE_BOUND ( 'NONE', #13882, .T. ) ;
#9835 = ORIENTED_EDGE ( 'NONE', *, *, #3267, .T. ) ;
#9836 = EDGE_LOOP ( 'NONE', ( #12180, #1561, #10300, #4937 ) ) ;
#9837 = AXIS2_PLACEMENT_3D ( 'NONE', #14135, #1829, #10451 ) ;
#9838 = CIRCLE ( 'NONE', #8668, 4.999999999999976907 ) ;
#9839 = ORIENTED_EDGE ( 'NONE', *, *, #7682, .F. ) ;
#9840 = CARTESIAN_POINT ( 'NONE',  ( 4.197393957002307552, 7.823395958202418729E-14, -3.203767560748914445 ) ) ;
#9841 = CYLINDRICAL_SURFACE ( 'NONE', #4951, 300.0000000000001137 ) ;
#9842 = ORIENTED_EDGE ( 'NONE', *, *, #3525, .F. ) ;
#9843 = CONICAL_SURFACE ( 'NONE', #10311, 5.000000000000000888, 0.9110539511682884672 ) ;
#9844 = DIRECTION ( 'NONE',  ( 0.000000000000000000, 0.000000000000000000, 1.000000000000000000 ) ) ;
#9845 = CARTESIAN_POINT ( 'NONE',  ( -3.999999999999996447, 0.7924765000094545764, -0.05906175389889514044 ) ) ;
#9846 = EDGE_CURVE ( 'NONE', #13192, #7349, #12841, .T. ) ;
#9847 = EDGE_CURVE ( 'NONE', #4128, #7846, #11743, .T. ) ;
#9848 = DIRECTION ( 'NONE',  ( 0.000000000000000000, 0.000000000000000000, 1.000000000000000000 ) ) ;
#9849 = CARTESIAN_POINT ( 'NONE',  ( -4.296971609536595516, 3.292644976429713655, -4.396693167835552529 ) ) ;
#9850 = EDGE_LOOP ( 'NONE', ( #11791, #14448, #7844, #11547, #13318 ) ) ;
#9851 =( NAMED_UNIT ( * ) PLANE_ANGLE_UNIT ( ) SI_UNIT ( $, .RADIAN. ) );
#9852 = EDGE_CURVE ( 'NONE', #5618, #45, #6171, .T. ) ;
#9853 = CARTESIAN_POINT ( 'NONE',  ( -4.000000000000000000, -2.309401076758511806, -3.133295621305376422 ) ) ;
#9854 = CIRCLE ( 'NONE', #3553, 2.500000000000002220 ) ;
#9855 = VECTOR ( 'NONE', #3602, 1000.000000000000000 ) ;
#9856 = FACE_OUTER_BOUND ( 'NONE', #12614, .T. ) ;
#9857 = B_SPLINE_CURVE_WITH_KNOTS ( 'NONE', 3,
 ( #3154, #6562, #5537, #7810, #11033, #12355 ),
 .UNSPECIFIED., .F., .F.,
 ( 4, 2, 4 ),
 ( 0.000000000000000000, 0.002086519881787261485, 0.004173039763574522103 ),
 .UNSPECIFIED. ) ;
#9858 = EDGE_LOOP ( 'NONE', ( #11043, #6372, #11589, #604 ) ) ;
#9859 = ADVANCED_FACE ( 'NONE', ( #14026 ), #3993, .T. ) ;
#9860 = ORIENTED_EDGE ( 'NONE', *, *, #10392, .T. ) ;
#9861 = ORIENTED_EDGE ( 'NONE', *, *, #5216, .F. ) ;
#9862 = DIRECTION ( 'NONE',  ( -1.000000000000000000, 0.000000000000000000, 0.000000000000000000 ) ) ;
#9863 = VECTOR ( 'NONE', #8810, 1000.000000000000000 ) ;
#9864 = ORIENTED_EDGE ( 'NONE', *, *, #11840, .T. ) ;
#9865 = CARTESIAN_POINT ( 'NONE',  ( 3.880198502136731786, 0.7307680362939255048, -3.499999999999992895 ) ) ;
#9866 = VECTOR ( 'NONE', #11684, 1000.000000000000000 ) ;
#9867 = CIRCLE ( 'NONE', #12913, 5.371010071662830399 ) ;
#9868 = ADVANCED_FACE ( 'NONE', ( #11819 ), #8137, .F. ) ;
#9869 = LINE ( 'NONE', #12208, #14036 ) ;
#9870 = EDGE_CURVE ( 'NONE', #14193, #8048, #6348, .T. ) ;
#9871 = DIRECTION ( 'NONE',  ( 1.000000000000000000, 0.000000000000000000, 0.000000000000000000 ) ) ;
#9872 = CARTESIAN_POINT ( 'NONE',  ( -31.44014396567295577, 38.31657438465165200, 8.000000000000007105 ) ) ;
#9873 = DIRECTION ( 'NONE',  ( 1.000000000000000000, 1.224646799147353454E-16, 0.000000000000000000 ) ) ;
#9874 = PRODUCT_CONTEXT ( 'NONE', #10544, 'mechanical' ) ;
#9875 = DIRECTION ( 'NONE',  ( 0.000000000000000000, 0.000000000000000000, 1.000000000000000000 ) ) ;
#9876 = CARTESIAN_POINT ( 'NONE',  ( 4.175075985190068728, 2.060370777630132544, -3.568666869285572307 ) ) ;
#9877 = ORIENTED_EDGE ( 'NONE', *, *, #1453, .T. ) ;
#9878 = VECTOR ( 'NONE', #4048, 1000.000000000000000 ) ;
#9879 = PLANE ( 'NONE',  #10348 ) ;
#9880 = VECTOR ( 'NONE', #3733, 1000.000000000000000 ) ;
#9881 = ORIENTED_EDGE ( 'NONE', *, *, #10976, .T. ) ;
#9882 = EDGE_CURVE ( 'NONE', #2918, #11701, #1690, .T. ) ;
#9883 = ORIENTED_EDGE ( 'NONE', *, *, #11206, .T. ) ;
#9884 = ORIENTED_EDGE ( 'NONE', *, *, #5138, .T. ) ;
#9885 = CARTESIAN_POINT ( 'NONE',  ( -5.253368672218636348, 3.033033817057773085, -4.659491423763650886 ) ) ;
#9886 = CARTESIAN_POINT ( 'NONE',  ( 19.99999999999999645, 57.00000000000000000, -25.00000000000000000 ) ) ;
#9887 = CIRCLE ( 'NONE', #4298, 3.499999999999999112 ) ;
#9888 = CARTESIAN_POINT ( 'NONE',  ( 4.847001880572344490, 3.878482749467366819, -1.282270821642922387 ) ) ;
#9889 = CARTESIAN_POINT ( 'NONE',  ( -2.450000000000000622, 3.000384657911016356E-16, -0.3851141460153306717 ) ) ;
#9890 = VERTEX_POINT ( 'NONE', #4362 ) ;
#9891 = CARTESIAN_POINT ( 'NONE',  ( 0.000000000000000000, 0.8660254037844428154, -1.500000000000001332 ) ) ;
#9892 = CARTESIAN_POINT ( 'NONE',  ( 20.00000000000000000, 5.000000000000000000, 25.00000000000000000 ) ) ;
#9893 = EDGE_CURVE ( 'NONE', #7396, #974, #3254, .T. ) ;
#9894 = CARTESIAN_POINT ( 'NONE',  ( -5.000000000000001776, -2.886751345948152192, -4.284345921091780696 ) ) ;
#9895 = AXIS2_PLACEMENT_3D ( 'NONE', #1852, #755, #7541 ) ;
#9896 = EDGE_LOOP ( 'NONE', ( #9540, #13640, #14404, #4461 ) ) ;
#9897 = DIRECTION ( 'NONE',  ( -2.081668171172169006E-16, 0.000000000000000000, -1.000000000000000000 ) ) ;
#9898 = VECTOR ( 'NONE', #2936, 1000.000000000000000 ) ;
#9899 = DIRECTION ( 'NONE',  ( -0.000000000000000000, 1.000000000000000000, -0.000000000000000000 ) ) ;
#9900 = CARTESIAN_POINT ( 'NONE',  ( 5.085009042717532957, -4.657032265668552995, -0.06621649662555413596 ) ) ;
#9901 = DIRECTION ( 'NONE',  ( 0.000000000000000000, 3.216245299353272708E-16, 1.000000000000000000 ) ) ;
#9902 = CARTESIAN_POINT ( 'NONE',  ( 31.80000000000005045, 6.938893903907228378E-15, 2.775557561562891351E-14 ) ) ;
#9903 = CARTESIAN_POINT ( 'NONE',  ( 108.6817075744280174, 109.5765550933605113, 3.300000000000008260 ) ) ;
#9904 = PRODUCT_DEFINITION_FORMATION_WITH_SPECIFIED_SOURCE ( 'ANY', '', #11629, .NOT_KNOWN. ) ;
#9905 = FACE_OUTER_BOUND ( 'NONE', #2156, .T. ) ;
#9906 = ORIENTED_EDGE ( 'NONE', *, *, #7534, .T. ) ;
#9907 = EDGE_LOOP ( 'NONE', ( #6093, #9086, #13776, #7782 ) ) ;
#9908 = CARTESIAN_POINT ( 'NONE',  ( 0.000000000000000000, 0.000000000000000000, 33.00000000000002842 ) ) ;
#9909 =( NAMED_UNIT ( * ) SI_UNIT ( $, .STERADIAN. ) SOLID_ANGLE_UNIT ( ) );
#9910 = AXIS2_PLACEMENT_3D ( 'NONE', #8531, #6533, #11003 ) ;
#9911 = ORIENTED_EDGE ( 'NONE', *, *, #8315, .T. ) ;
#9912 = CARTESIAN_POINT ( 'NONE',  ( 58.68170757442803165, -83.66032599071898801, 28.00000000000000000 ) ) ;
#9913 = ADVANCED_FACE ( 'NONE', ( #12101 ), #5421, .T. ) ;
#9914 = FACE_BOUND ( 'NONE', #9144, .T. ) ;
#9915 = PRODUCT_RELATED_PRODUCT_CATEGORY ( 'part', '', ( #3937 ) ) ;
#9916 = EDGE_CURVE ( 'NONE', #13539, #5373, #4216, .T. ) ;
#9917 = ORIENTED_EDGE ( 'NONE', *, *, #14217, .T. ) ;
#9918 = EDGE_LOOP ( 'NONE', ( #33, #11862, #9483, #6089 ) ) ;
#9919 = CARTESIAN_POINT ( 'NONE',  ( -3.510273485745311284, -2.827716139362665082, -3.310536846335872418 ) ) ;
#9920 = DIRECTION ( 'NONE',  ( 1.000000000000000000, 0.000000000000000000, 0.000000000000000000 ) ) ;
#9921 = CARTESIAN_POINT ( 'NONE',  ( 4.030867648405854098, 2.329326259789020526, -2.965488570641532373 ) ) ;
#9922 = DIRECTION ( 'NONE',  ( 0.000000000000000000, 0.000000000000000000, -1.000000000000000000 ) ) ;
#9923 = CARTESIAN_POINT ( 'NONE',  ( 1.560000000000005826, 0.8660254037844428154, 1.500000000000001332 ) ) ;
#9924 = VECTOR ( 'NONE', #10968, 1000.000000000000000 ) ;
#9925 =( BOUNDED_SURFACE ( )  B_SPLINE_SURFACE ( 3, 2, ( 
 ( #8219, #13669, #2753 ),
 ( #1566, #5016, #12845 ),
 ( #7271, #10497, #8068 ),
 ( #12688, #4794, #1501 ),
 ( #6971, #6014, #7192 ),
 ( #7045, #7118, #10573 ) ),
 .UNSPECIFIED., .F., .F., .T. ) 
 B_SPLINE_SURFACE_WITH_KNOTS ( ( 4, 2, 4 ),
 ( 3, 3 ),
 ( 0.02023740217035200836, 0.02269762987400599299, 0.02515785757765997763 ),
 ( 0.000000000000000000, 1.000000000000000000 ),
 .UNSPECIFIED. ) 
 GEOMETRIC_REPRESENTATION_ITEM ( )  RATIONAL_B_SPLINE_SURFACE ( (
 ( 1.000000000000000000, 0.8047781539129733597, 1.000000000000000000),
 ( 1.000000000000000000, 0.8123770319057124212, 1.000000000000000000),
 ( 1.000000000000000000, 0.8190663783056869596, 1.000000000000000000),
 ( 1.000000000000000000, 0.8192359702877044514, 1.000000000000000000),
 ( 1.000000000000000000, 0.8126134888419825897, 1.000000000000000000),
 ( 1.000000000000000000, 0.8047712368238113534, 1.000000000000000000) ) ) 
 REPRESENTATION_ITEM ( '' )  SURFACE ( )  );
#9926 = CARTESIAN_POINT ( 'NONE',  ( 20.00000000000000711, 20.00000000000000355, 25.00000000000000000 ) ) ;
#9927 = DIRECTION ( 'NONE',  ( -1.913084959030911013E-15, 1.000000000000000000, 0.000000000000000000 ) ) ;
#9928 = CARTESIAN_POINT ( 'NONE',  ( 54.35294117647056567, -1.411764705882362358, -25.00000000000000000 ) ) ;
#9929 = LINE ( 'NONE', #997, #13269 ) ;
#9930 = VERTEX_POINT ( 'NONE', #3117 ) ;
#9931 = VERTEX_POINT ( 'NONE', #14164 ) ;
#9932 = ORIENTED_EDGE ( 'NONE', *, *, #13707, .F. ) ;
#9933 = CARTESIAN_POINT ( 'NONE',  ( 0.000000000000000000, 0.000000000000000000, -4.699999999999981526 ) ) ;
#9934 = VERTEX_POINT ( 'NONE', #6446 ) ;
#9935 = DIRECTION ( 'NONE',  ( 0.000000000000000000, 0.000000000000000000, -1.000000000000000000 ) ) ;
#9936 = LINE ( 'NONE', #6349, #9573 ) ;
#9937 = CARTESIAN_POINT ( 'NONE',  ( 56.83050351964436686, 32.98574998546678927, 25.00000000000000000 ) ) ;
#9938 = LINE ( 'NONE', #5327, #10699 ) ;
#9939 = ORIENTED_EDGE ( 'NONE', *, *, #2799, .F. ) ;
#9940 = DIRECTION ( 'NONE',  ( 0.000000000000000000, 0.000000000000000000, -1.000000000000000000 ) ) ;
#9941 = CARTESIAN_POINT ( 'NONE',  ( 3.999999999999998224, -0.8577736050348424568, -3.133260139357294083 ) ) ;
#9942 = CARTESIAN_POINT ( 'NONE',  ( 4.142654963991840411, 2.035398498734362072, -3.525413613457308859 ) ) ;
#9943 = ORIENTED_EDGE ( 'NONE', *, *, #11083, .F. ) ;
#9944 = DIRECTION ( 'NONE',  ( 0.000000000000000000, 0.000000000000000000, 1.000000000000000000 ) ) ;
#9945 = EDGE_CURVE ( 'NONE', #8749, #2554, #14379, .T. ) ;
#9946 = ORIENTED_EDGE ( 'NONE', *, *, #3432, .T. ) ;
#9947 = EDGE_CURVE ( 'NONE', #6958, #3442, #8797, .T. ) ;
#9948 = ORIENTED_EDGE ( 'NONE', *, *, #2177, .F. ) ;
#9949 = ORIENTED_EDGE ( 'NONE', *, *, #13537, .T. ) ;
#9950 = VECTOR ( 'NONE', #101, 1000.000000000000000 ) ;
#9951 = ORIENTED_EDGE ( 'NONE', *, *, #12936, .F. ) ;
#9952 = FACE_OUTER_BOUND ( 'NONE', #13777, .T. ) ;
#9953 = CARTESIAN_POINT ( 'NONE',  ( 0.000000000000000000, 0.000000000000000000, 0.000000000000000000 ) ) ;
#9954 = CARTESIAN_POINT ( 'NONE',  ( 57.35294117647057277, -1.411764705882362358, 25.00000000000000000 ) ) ;
#9955 = LINE ( 'NONE', #4345, #1190 ) ;
#9956 = ORIENTED_EDGE ( 'NONE', *, *, #4936, .T. ) ;
#9957 = CARTESIAN_POINT ( 'NONE',  ( 20.00000000000000000, -5.510910596163090344E-15, 25.00000000000000000 ) ) ;
#9958 = DIRECTION ( 'NONE',  ( 0.000000000000000000, 0.000000000000000000, -1.000000000000000000 ) ) ;
#9959 = DIRECTION ( 'NONE',  ( 0.000000000000000000, 0.000000000000000000, 1.000000000000000000 ) ) ;
#9960 = EDGE_CURVE ( 'NONE', #1865, #4996, #2971, .T. ) ;
#9961 = CARTESIAN_POINT ( 'NONE',  ( 88.22284556172391490, -83.66032599071898801, 28.00000000000000000 ) ) ;
#9962 = ORIENTED_EDGE ( 'NONE', *, *, #12092, .T. ) ;
#9963 = DIRECTION ( 'NONE',  ( 0.000000000000000000, 0.000000000000000000, -1.000000000000000000 ) ) ;
#9964 = FACE_OUTER_BOUND ( 'NONE', #3131, .T. ) ;
#9965 = ADVANCED_FACE ( 'NONE', ( #8656, #9905 ), #7694, .F. ) ;
#9966 = DIRECTION ( 'NONE',  ( 0.000000000000000000, 0.000000000000000000, 1.000000000000000000 ) ) ;
#9967 = ORIENTED_EDGE ( 'NONE', *, *, #2311, .T. ) ;
#9968 = LINE ( 'NONE', #2221, #4932 ) ;
#9969 = CARTESIAN_POINT ( 'NONE',  ( 4.988724804725785944, -2.309401076758511806, -3.999999999999989786 ) ) ;
#9970 = LINE ( 'NONE', #6594, #1779 ) ;
#9971 = DIRECTION ( 'NONE',  ( 0.000000000000000000, 0.000000000000000000, -1.000000000000000000 ) ) ;
#9972 = CARTESIAN_POINT ( 'NONE',  ( 4.175813232069169878, -4.122719923832743660, -6.938893903907228378E-15 ) ) ;
#9973 =( LENGTH_UNIT ( ) NAMED_UNIT ( * ) SI_UNIT ( .MILLI., .METRE. ) );
#9974 = ADVANCED_FACE ( 'NONE', ( #3183 ), #10716, .T. ) ;
#9975 = CARTESIAN_POINT ( 'NONE',  ( 4.939011777414161308, 1.602816961020108844, 4.000000000000002665 ) ) ;
#9976 = VERTEX_POINT ( 'NONE', #10990 ) ;
#9977 = AXIS2_PLACEMENT_3D ( 'NONE', #3388, #2274, #11190 ) ;
#9978 = EDGE_LOOP ( 'NONE', ( #7184, #5996 ) ) ;
#9979 = CARTESIAN_POINT ( 'NONE',  ( 5.000000000000001776, -1.387778780781445676E-14, -3.920524600599840426 ) ) ;
#9980 = PLANE ( 'NONE',  #5307 ) ;
#9981 = CARTESIAN_POINT ( 'NONE',  ( -118.6817075744283727, 189.5765550933606107, 33.00000000000002842 ) ) ;
#9982 = ORIENTED_EDGE ( 'NONE', *, *, #589, .F. ) ;
#9983 = VECTOR ( 'NONE', #12832, 1000.000000000000000 ) ;
#9984 = B_SPLINE_CURVE_WITH_KNOTS ( 'NONE', 3,
 ( #12560, #3871, #2403, #3586 ),
 .UNSPECIFIED., .F., .F.,
 ( 4, 4 ),
 ( 0.002376763279741535111, 0.004766460739942319363 ),
 .UNSPECIFIED. ) ;
#9985 = ORIENTED_EDGE ( 'NONE', *, *, #13152, .T. ) ;
#9986 = ORIENTED_EDGE ( 'NONE', *, *, #7232, .T. ) ;
#9987 = FACE_BOUND ( 'NONE', #9615, .T. ) ;
#9988 = CARTESIAN_POINT ( 'NONE',  ( 20.00000000000000000, 27.00000000000000355, -25.00000000000000000 ) ) ;
#9989 =( REPRESENTATION_RELATIONSHIP ('NONE','NONE', #10295, #7389 ) REPRESENTATION_RELATIONSHIP_WITH_TRANSFORMATION ( #11034 )SHAPE_REPRESENTATION_RELATIONSHIP( ) );
#9990 = VECTOR ( 'NONE', #2527, 1000.000000000000114 ) ;
#9991 = PLANE ( 'NONE',  #12868 ) ;
#9992 = CARTESIAN_POINT ( 'NONE',  ( 0.000000000000000000, 40.49999999999999289, 0.000000000000000000 ) ) ;
#9993 = FACE_OUTER_BOUND ( 'NONE', #5872, .T. ) ;
#9994 = ADVANCED_FACE ( 'NONE', ( #8728 ), #1862, .T. ) ;
#9995 = DIRECTION ( 'NONE',  ( 1.000000000000000000, 1.665334536937733825E-16, 0.000000000000000000 ) ) ;
#9996 = DIRECTION ( 'NONE',  ( -1.000000000000000000, -3.286707217423839940E-17, -2.273843122241288053E-18 ) ) ;
#9997 = DIRECTION ( 'NONE',  ( 1.000000000000000000, 0.000000000000000000, 0.000000000000000000 ) ) ;
#9998 = ORIENTED_EDGE ( 'NONE', *, *, #8784, .F. ) ;
#9999 = EDGE_LOOP ( 'NONE', ( #14114, #9682, #13602, #11045 ) ) ;
#10000 = EDGE_LOOP ( 'NONE', ( #6252, #12504, #6020, #8247 ) ) ;
#10001 = DIRECTION ( 'NONE',  ( -1.000000000000000000, 0.000000000000000000, 0.000000000000000000 ) ) ;
#10002 = ORIENTED_EDGE ( 'NONE', *, *, #742, .T. ) ;
#10003 = DIRECTION ( 'NONE',  ( 0.000000000000000000, -1.000000000000000000, 0.000000000000000000 ) ) ;
#10004 = LINE ( 'NONE', #10826, #3732 ) ;
#10005 = CIRCLE ( 'NONE', #14454, 8.000000000000000000 ) ;
#10006 = FACE_OUTER_BOUND ( 'NONE', #1846, .T. ) ;
#10007 = CARTESIAN_POINT ( 'NONE',  ( 108.6817075744280743, 59.57655509336061073, 25.00000000000000000 ) ) ;
#10008 = VECTOR ( 'NONE', #10433, 1000.000000000000000 ) ;
#10009 = DIRECTION ( 'NONE',  ( -0.000000000000000000, -0.000000000000000000, -1.000000000000000000 ) ) ;
#10010 = CARTESIAN_POINT ( 'NONE',  ( 21.68170757442799967, 141.2731697022880155, -28.00000000000000000 ) ) ;
#10011 = FACE_OUTER_BOUND ( 'NONE', #9220, .T. ) ;
#10012 = ADVANCED_FACE ( 'NONE', ( #7405 ), #11963, .F. ) ;
#10013 = LINE ( 'NONE', #12075, #1708 ) ;
#10014 = VERTEX_POINT ( 'NONE', #13146 ) ;
#10015 = STYLED_ITEM ( 'NONE', ( #2927 ), #6873 ) ;
#10016 = VERTEX_POINT ( 'NONE', #12035 ) ;
#10017 = ORIENTED_EDGE ( 'NONE', *, *, #14296, .F. ) ;
#10018 = ORIENTED_EDGE ( 'NONE', *, *, #4337, .F. ) ;
#10019 = CARTESIAN_POINT ( 'NONE',  ( 20.00000000000000000, 80.00000000000000000, 25.00000000000000000 ) ) ;
#10020 = FILL_AREA_STYLE ('',( #4414 ) ) ;
#10021 = CARTESIAN_POINT ( 'NONE',  ( 0.000000000000000000, 0.000000000000000000, -4.184454397937131809 ) ) ;
#10022 = EDGE_LOOP ( 'NONE', ( #6337, #2532 ) ) ;
#10023 = CARTESIAN_POINT ( 'NONE',  ( 25.00000000000000000, 199.5765550933606107, 47.99999999999998579 ) ) ;
#10024 = CARTESIAN_POINT ( 'NONE',  ( 4.000000000000003553, -2.309401076758511806, -3.133295621305376422 ) ) ;
#10025 = EDGE_CURVE ( 'NONE', #4996, #1788, #894, .T. ) ;
#10026 = FACE_OUTER_BOUND ( 'NONE', #13040, .T. ) ;
#10027 = ORIENTED_EDGE ( 'NONE', *, *, #5814, .T. ) ;
#10028 = ADVANCED_FACE ( 'NONE', ( #9824 ), #14099, .T. ) ;
#10029 = ORIENTED_EDGE ( 'NONE', *, *, #2016, .T. ) ;
#10030 = CARTESIAN_POINT ( 'NONE',  ( 32.57694101601105530, 130.0000000000000000, 25.00000000000000000 ) ) ;
#10031 = PLANE ( 'NONE',  #6360 ) ;
#10032 = EDGE_CURVE ( 'NONE', #9244, #7329, #6819, .T. ) ;
#10033 = DIRECTION ( 'NONE',  ( -1.000000000000000000, 2.551526159633733968E-19, 1.987661601597216239E-18 ) ) ;
#10034 = VERTEX_POINT ( 'NONE', #8580 ) ;
#10035 = DIRECTION ( 'NONE',  ( 0.000000000000000000, 0.000000000000000000, 1.000000000000000000 ) ) ;
#10036 = EDGE_CURVE ( 'NONE', #7552, #11916, #51, .T. ) ;
#10037 = AXIS2_PLACEMENT_3D ( 'NONE', #10076, #6703, #11172 ) ;
#10038 = CARTESIAN_POINT ( 'NONE',  ( 0.3126073911696169993, -2.020725942163681399, 3.499999999999989342 ) ) ;
#10039 = CARTESIAN_POINT ( 'NONE',  ( 1.560000000000005826, 0.8660254037844428154, 1.500000000000001332 ) ) ;
#10040 = CARTESIAN_POINT ( 'NONE',  ( 88.22284556172391490, 39.57655509336063915, -106.9999999999999858 ) ) ;
#10041 = AXIS2_PLACEMENT_3D ( 'NONE', #12228, #5277, #7529 ) ;
#10042 = EDGE_CURVE ( 'NONE', #8048, #14193, #525, .T. ) ;
#10043 = CARTESIAN_POINT ( 'NONE',  ( 5.013196232911362848, 2.310564645009344442, 4.002015359328507493 ) ) ;
#10044 = ORIENTED_EDGE ( 'NONE', *, *, #9473, .T. ) ;
#10045 = ORIENTED_EDGE ( 'NONE', *, *, #1919, .F. ) ;
#10046 = CARTESIAN_POINT ( 'NONE',  ( 2.000000000000015543, 3.464101615137753942, 0.000000000000000000 ) ) ;
#10047 = AXIS2_PLACEMENT_3D ( 'NONE', #11997, #725, #2034 ) ;
#10048 = EDGE_LOOP ( 'NONE', ( #6705, #13129, #12104, #9932 ) ) ;
#10049 = EDGE_CURVE ( 'NONE', #14160, #7658, #12823, .T. ) ;
#10050 = DIRECTION ( 'NONE',  ( 0.000000000000000000, -0.000000000000000000, 1.000000000000000000 ) ) ;
#10051 = ORIENTED_EDGE ( 'NONE', *, *, #2177, .T. ) ;
#10052 = ORIENTED_EDGE ( 'NONE', *, *, #12291, .T. ) ;
#10053 = ADVANCED_FACE ( 'NONE', ( #11075 ), #12434, .T. ) ;
#10054 = ORIENTED_EDGE ( 'NONE', *, *, #327, .T. ) ;
#10055 = DIRECTION ( 'NONE',  ( -1.000000000000000000, -4.406877377903811104E-17, 0.000000000000000000 ) ) ;
#10056 = CARTESIAN_POINT ( 'NONE',  ( -4.379424050594064255, -3.527728022193145296, -4.490801088233112637 ) ) ;
#10057 = CARTESIAN_POINT ( 'NONE',  ( 3.880206590543186618, -2.665671387532548398, -2.382921720511017583 ) ) ;
#10058 = CARTESIAN_POINT ( 'NONE',  ( 20.00000000000000000, -5.510910596163090344E-15, 25.00000000000000000 ) ) ;
#10059 = FACE_OUTER_BOUND ( 'NONE', #11345, .T. ) ;
#10060 = CARTESIAN_POINT ( 'NONE',  ( 5.000000000000000000, -2.886751345948148639, -6.000000000000005329 ) ) ;
#10061 = EDGE_LOOP ( 'NONE', ( #492, #12040 ) ) ;
#10062 = VERTEX_POINT ( 'NONE', #4825 ) ;
#10063 = CARTESIAN_POINT ( 'NONE',  ( 20.00000000000000000, -5.510910596163090344E-15, -25.00000000000000000 ) ) ;
#10064 = CARTESIAN_POINT ( 'NONE',  ( 13.00000000000000533, 29.99999999999999289, 8.000000000000007105 ) ) ;
#10065 = VECTOR ( 'NONE', #7586, 1000.000000000000000 ) ;
#10066 = VECTOR ( 'NONE', #2520, 1000.000000000000000 ) ;
#10067 = VERTEX_POINT ( 'NONE', #9289 ) ;
#10068 = VERTEX_POINT ( 'NONE', #4508 ) ;
#10069 = ADVANCED_FACE ( 'NONE', ( #1191 ), #7941, .F. ) ;
#10070 = CIRCLE ( 'NONE', #13125, 2.500000000000002220 ) ;
#10071 = VERTEX_POINT ( 'NONE', #445 ) ;
#10072 = CARTESIAN_POINT ( 'NONE',  ( 105.6817075744280174, 69.57655509336049704, 3.300000000000013589 ) ) ;
#10073 = ORIENTED_EDGE ( 'NONE', *, *, #685, .F. ) ;
#10074 = CARTESIAN_POINT ( 'NONE',  ( 4.052416734886548078, -1.393505408944210266, -3.567979131523931091 ) ) ;
#10075 = CARTESIAN_POINT ( 'NONE',  ( 5.000000000000001776, 1.044497431481508531, -4.017831869288535529 ) ) ;
#10076 = CARTESIAN_POINT ( 'NONE',  ( 21.68170757442808849, 141.2731697022877313, -23.00000000000000000 ) ) ;
#10077 = VECTOR ( 'NONE', #6211, 1000.000000000000000 ) ;
#10078 = CARTESIAN_POINT ( 'NONE',  ( -129.3408537872145132, 199.5765550933606107, -9.000000000000007105 ) ) ;
#10079 =( GEOMETRIC_REPRESENTATION_CONTEXT ( 3 ) GLOBAL_UNCERTAINTY_ASSIGNED_CONTEXT ( ( #5141 ) ) GLOBAL_UNIT_ASSIGNED_CONTEXT ( ( #4992, #13781, #9452 ) ) REPRESENTATION_CONTEXT ( 'NONE', 'WORKASPACE' ) );
#10080 = VECTOR ( 'NONE', #11057, 1000.000000000000000 ) ;
#10081 = LINE ( 'NONE', #7584, #6569 ) ;
#10082 = ITEM_DEFINED_TRANSFORMATION ( 'NONE', 'NONE', #11074,  #11025 ) ;
#10083 = CARTESIAN_POINT ( 'NONE',  ( 5.013196232911366401, -4.621129290018641811, -2.775422584047554243E-14 ) ) ;
#10084 = CARTESIAN_POINT ( 'NONE',  ( 4.132952817037849336, -2.031684012687273722, 3.518979934899753470 ) ) ;
#10085 = EDGE_LOOP ( 'NONE', ( #12414, #9877, #5121, #8968 ) ) ;
#10086 = EDGE_CURVE ( 'NONE', #8838, #1328, #9386, .T. ) ;
#10087 = AXIS2_PLACEMENT_3D ( 'NONE', #5475, #6709, #4474 ) ;
#10088 = AXIS2_PLACEMENT_3D ( 'NONE', #7734, #6423, #2114 ) ;
#10089 = EDGE_CURVE ( 'NONE', #12991, #12769, #8796, .T. ) ;
#10090 = CARTESIAN_POINT ( 'NONE',  ( 32.60000000000000142, 29.99999999999999645, -24.99999999999999289 ) ) ;
#10091 = ORIENTED_EDGE ( 'NONE', *, *, #13533, .F. ) ;
#10092 = ORIENTED_EDGE ( 'NONE', *, *, #2139, .T. ) ;
#10093 = CARTESIAN_POINT ( 'NONE',  ( 53.99999999999997868, -1.324077043022348342E-15, -23.00000000000000000 ) ) ;
#10094 = CARTESIAN_POINT ( 'NONE',  ( 58.68170757442803165, 39.57655509336063204, -33.00000000000000000 ) ) ;
#10095 = FILL_AREA_STYLE_COLOUR ( '', #5006 ) ;
#10096 = CARTESIAN_POINT ( 'NONE',  ( 19.99999999999999645, 57.00000000000000000, -25.00000000000000000 ) ) ;
#10097 = FACE_OUTER_BOUND ( 'NONE', #6313, .T. ) ;
#10098 = DIRECTION ( 'NONE',  ( -0.8660254037844381525, -0.5000000000000008882, 0.000000000000000000 ) ) ;
#10099 = DIRECTION ( 'NONE',  ( 1.000000000000000000, 0.000000000000000000, 0.000000000000000000 ) ) ;
#10100 = FACE_OUTER_BOUND ( 'NONE', #1246, .T. ) ;
#10101 = VERTEX_POINT ( 'NONE', #1050 ) ;
#10102 = VECTOR ( 'NONE', #2422, 1000.000000000000000 ) ;
#10103 = PRODUCT_DEFINITION_SHAPE ( 'NONE', 'NONE',  #14475 ) ;
#10104 = CARTESIAN_POINT ( 'NONE',  ( 6.938893903907228378E-15, 24.50000000000002132, 0.000000000000000000 ) ) ;
#10105 = FACE_OUTER_BOUND ( 'NONE', #10000, .T. ) ;
#10106 = ADVANCED_BREP_SHAPE_REPRESENTATION ( '', ( #11661, #11025 ), #1942 ) ;
#10107 = ORIENTED_EDGE ( 'NONE', *, *, #10963, .F. ) ;
#10108 = PRODUCT_DEFINITION_CONTEXT ( 'detailed design', #8089, 'design' ) ;
#10109 = CIRCLE ( 'NONE', #11762, 2.749999999999997780 ) ;
#10110 = LINE ( 'NONE', #14298, #5963 ) ;
#10111 = DIRECTION ( 'NONE',  ( 1.000000000000000000, 0.000000000000000000, 0.000000000000000000 ) ) ;
#10112 = FACE_OUTER_BOUND ( 'NONE', #7588, .T. ) ;
#10113 =( NAMED_UNIT ( * ) SI_UNIT ( $, .STERADIAN. ) SOLID_ANGLE_UNIT ( ) );
#10114 = DIRECTION ( 'NONE',  ( 0.000000000000000000, 0.000000000000000000, 1.000000000000000000 ) ) ;
#10115 = ORIENTED_EDGE ( 'NONE', *, *, #12539, .T. ) ;
#10116 = AXIS2_PLACEMENT_3D ( 'NONE', #6961, #12469, #4716 ) ;
#10117 = CARTESIAN_POINT ( 'NONE',  ( 22.00000000000000000, 70.00000000000000000, -25.00000000000000000 ) ) ;
#10118 = EDGE_CURVE ( 'NONE', #5057, #6958, #9359, .T. ) ;
#10119 = VECTOR ( 'NONE', #7397, 1000.000000000000114 ) ;
#10120 = SHAPE_REPRESENTATION_RELATIONSHIP ( 'NONE' , 'NONE' ,  #5343, #1042 ) ;
#10121 = EDGE_LOOP ( 'NONE', ( #13710, #9216, #11437, #6133 ) ) ;
#10122 = DIRECTION ( 'NONE',  ( 0.000000000000000000, 0.000000000000000000, -1.000000000000000000 ) ) ;
#10123 = CIRCLE ( 'NONE', #319, 2.500000000000002220 ) ;
#10124 = ADVANCED_FACE ( 'NONE', ( #3819 ), #12169, .F. ) ;
#10125 = EDGE_CURVE ( 'NONE', #1916, #4911, #2885, .T. ) ;
#10126 = ORIENTED_EDGE ( 'NONE', *, *, #11936, .T. ) ;
#10127 = FACE_OUTER_BOUND ( 'NONE', #8008, .T. ) ;
#10128 = FACE_OUTER_BOUND ( 'NONE', #4643, .T. ) ;
#10129 = PRODUCT_DEFINITION_FORMATION_WITH_SPECIFIED_SOURCE ( 'ANY', '', #3937, .NOT_KNOWN. ) ;
#10130 = CARTESIAN_POINT ( 'NONE',  ( 3.958484000406985004, 2.327740518748977028, -2.968235154690041178 ) ) ;
#10131 = DIRECTION ( 'NONE',  ( 0.000000000000000000, 0.000000000000000000, 1.000000000000000000 ) ) ;
#10132 =( NAMED_UNIT ( * ) SI_UNIT ( $, .STERADIAN. ) SOLID_ANGLE_UNIT ( ) );
#10133 = CARTESIAN_POINT ( 'NONE',  ( 4.071447262713911996, 2.020725942163681399, -3.499999999999996003 ) ) ;
#10134 = B_SPLINE_CURVE_WITH_KNOTS ( 'NONE', 3,
 ( #1301, #13475, #7891, #4412, #5688, #8844, #2337, #148, #4615, #9056 ),
 .UNSPECIFIED., .F., .F.,
 ( 4, 2, 2, 2, 4 ),
 ( 0.000000000000000000, 0.001528561485809835615, 0.003057122971619672530, 0.004585684457429509663, 0.006114245943239346795 ),
 .UNSPECIFIED. ) ;
#10135 = LINE ( 'NONE', #6757, #13065 ) ;
#10136 = VERTEX_POINT ( 'NONE', #9586 ) ;
#10137 = DIRECTION ( 'NONE',  ( -2.273843122241288438E-18, -5.551115123125783935E-17, -1.000000000000000000 ) ) ;
#10138 = AXIS2_PLACEMENT_3D ( 'NONE', #3363, #5599, #1432 ) ;
#10139 = ORIENTED_EDGE ( 'NONE', *, *, #14050, .T. ) ;
#10140 = LINE ( 'NONE', #11232, #5348 ) ;
#10141 = EDGE_CURVE ( 'NONE', #9934, #12581, #1685, .T. ) ;
#10142 = CYLINDRICAL_SURFACE ( 'NONE', #4172, 5.000000000000004441 ) ;
#10143 = CARTESIAN_POINT ( 'NONE',  ( 59.25585977000769589, 23.28432498401347672, 25.00000000000000000 ) ) ;
#10144 = ORIENTED_EDGE ( 'NONE', *, *, #10256, .F. ) ;
#10145 = B_SPLINE_CURVE_WITH_KNOTS ( 'NONE', 3,
 ( #8670, #13158, #13442, #5581, #5781, #38 ),
 .UNSPECIFIED., .F., .F.,
 ( 4, 2, 4 ),
 ( 0.002950759650825642358, 0.004429055062152263689, 0.005907350473478885887 ),
 .UNSPECIFIED. ) ;
#10146 = EDGE_LOOP ( 'NONE', ( #8150, #13735, #14347, #10933 ) ) ;
#10147 = ORIENTED_EDGE ( 'NONE', *, *, #2926, .T. ) ;
#10148 = LINE ( 'NONE', #9033, #7801 ) ;
#10149 = ORIENTED_EDGE ( 'NONE', *, *, #10577, .F. ) ;
#10150 = LINE ( 'NONE', #2256, #10973 ) ;
#10151 = LINE ( 'NONE', #8900, #201 ) ;
#10152 = DIRECTION ( 'NONE',  ( -1.000000000000000000, -3.286707217423839940E-17, -2.273843122241288053E-18 ) ) ;
#10153 = DIRECTION ( 'NONE',  ( 0.000000000000000000, 0.000000000000000000, 1.000000000000000000 ) ) ;
#10154 = DIRECTION ( 'NONE',  ( 0.2425356250363328581, -0.9701425001453318764, -0.000000000000000000 ) ) ;
#10155 = ITEM_DEFINED_TRANSFORMATION ( 'NONE', 'NONE', #2203,  #11025 ) ;
#10156 = CARTESIAN_POINT ( 'NONE',  ( 0.000000000000000000, 3.031088913245522320, 1.750000000000001554 ) ) ;
#10157 = ADVANCED_FACE ( 'NONE', ( #10615, #7230, #600, #2945, #13038 ), #4120, .F. ) ;
#10158 = DIRECTION ( 'NONE',  ( -1.000000000000000000, 0.000000000000000000, 0.000000000000000000 ) ) ;
#10159 = CARTESIAN_POINT ( 'NONE',  ( 5.005210273051233116, 2.263846804438351512, 4.078902314160334441 ) ) ;
#10160 = ORIENTED_EDGE ( 'NONE', *, *, #3346, .F. ) ;
#10161 = ADVANCED_FACE ( 'NONE', ( #10831 ), #11787, .T. ) ;
#10162 = CARTESIAN_POINT ( 'NONE',  ( -2.725758460534058791, 3.045084772581766686, -2.920601398289325079 ) ) ;
#10163 = VERTEX_POINT ( 'NONE', #805 ) ;
#10164 = ORIENTED_EDGE ( 'NONE', *, *, #3800, .F. ) ;
#10165 = CARTESIAN_POINT ( 'NONE',  ( 0.000000000000000000, 0.000000000000000000, -4.184454397937131809 ) ) ;
#10166 = DIRECTION ( 'NONE',  ( 1.892425610156517122E-16, 1.000000000000000000, 0.000000000000000000 ) ) ;
#10167 = CARTESIAN_POINT ( 'NONE',  ( 3.680118525130247065, -2.494084732383348602, -0.3507732604232590701 ) ) ;
#10168 = CARTESIAN_POINT ( 'NONE',  ( 0.000000000000000000, 17.49899999999995970, 4.000000000000003553 ) ) ;
#10169 = CARTESIAN_POINT ( 'NONE',  ( 2.949999999999994404, 0.000000000000000000, 2.699999999999999289 ) ) ;
#10170 = SURFACE_STYLE_USAGE ( .BOTH. , #3390 ) ;
#10171 = EDGE_CURVE ( 'NONE', #10589, #12756, #2181, .T. ) ;
#10172 = CARTESIAN_POINT ( 'NONE',  ( -4.000000000000000000, -1.762750951161524442E-16, 1.599999999999990319 ) ) ;
#10173 = ORIENTED_EDGE ( 'NONE', *, *, #299, .T. ) ;
#10174 = EDGE_CURVE ( 'NONE', #6239, #13071, #9150, .T. ) ;
#10175 = CARTESIAN_POINT ( 'NONE',  ( 0.1586754815284818487, -4.240386000424023472, -0.6554360035618013169 ) ) ;
#10176 = VERTEX_POINT ( 'NONE', #672 ) ;
#10177 = PLANE ( 'NONE',  #615 ) ;
#10178 = DIRECTION ( 'NONE',  ( -1.000000000000000000, 0.000000000000000000, 0.000000000000000000 ) ) ;
#10179 = PLANE ( 'NONE',  #3276 ) ;
#10180 = ORIENTED_EDGE ( 'NONE', *, *, #14076, .T. ) ;
#10181 = VERTEX_POINT ( 'NONE', #4040 ) ;
#10182 = ADVANCED_FACE ( 'NONE', ( #5049 ), #7312, .F. ) ;
#10183 = ORIENTED_EDGE ( 'NONE', *, *, #8071, .T. ) ;
#10184 = DIRECTION ( 'NONE',  ( -1.000000000000000000, 0.000000000000000000, 0.000000000000000000 ) ) ;
#10185 = ORIENTED_EDGE ( 'NONE', *, *, #5552, .F. ) ;
#10186 = CARTESIAN_POINT ( 'NONE',  ( 4.538180240577822737E-16, 3.070647092368435693, 2.681483223904234325 ) ) ;
#10187 = ADVANCED_FACE ( 'NONE', ( #14067 ), #13986, .F. ) ;
#10188 = DIRECTION ( 'NONE',  ( -4.406877377903809255E-17, 1.000000000000000000, 0.000000000000000000 ) ) ;
#10189 = CARTESIAN_POINT ( 'NONE',  ( -5.253368672218639013, -3.033033817057793957, -4.659491423763650886 ) ) ;
#10190 = LINE ( 'NONE', #2377, #9357 ) ;
#10191 = DIRECTION ( 'NONE',  ( 1.000000000000000000, 3.286707217423839940E-17, 2.273843122241288053E-18 ) ) ;
#10192 = AXIS2_PLACEMENT_3D ( 'NONE', #10168, #3451, #1247 ) ;
#10193 = CARTESIAN_POINT ( 'NONE',  ( 3.951447005078473573, 3.704664227300106916, -0.5833333333333333703 ) ) ;
#10194 = VERTEX_POINT ( 'NONE', #519 ) ;
#10195 = CARTESIAN_POINT ( 'NONE',  ( 0.03111943836866626692, 6.084399642271180575, -4.666192694417975240 ) ) ;
#10196 = EDGE_CURVE ( 'NONE', #13520, #8214, #9867, .T. ) ;
#10197 = ORIENTED_EDGE ( 'NONE', *, *, #2136, .F. ) ;
#10198 = DIRECTION ( 'NONE',  ( 0.000000000000000000, 0.000000000000000000, -1.000000000000000000 ) ) ;
#10199 = ORIENTED_EDGE ( 'NONE', *, *, #589, .T. ) ;
#10200 = DIRECTION ( 'NONE',  ( -1.000000000000000000, -1.723842398015259277E-15, 0.000000000000000000 ) ) ;
#10201 = EDGE_CURVE ( 'NONE', #14013, #5279, #11930, .T. ) ;
#10202 = ORIENTED_EDGE ( 'NONE', *, *, #2359, .T. ) ;
#10203 = ADVANCED_FACE ( 'NONE', ( #1903 ), #13919, .T. ) ;
#10204 = ORIENTED_EDGE ( 'NONE', *, *, #6735, .T. ) ;
#10205 = AXIS2_PLACEMENT_3D ( 'NONE', #7350, #11668, #13949 ) ;
#10206 = ORIENTED_EDGE ( 'NONE', *, *, #14204, .F. ) ;
#10207 = VECTOR ( 'NONE', #12859, 1000.000000000000000 ) ;
#10208 = CARTESIAN_POINT ( 'NONE',  ( 30.07694101601105530, 130.0000000000000000, 25.00000000000000000 ) ) ;
#10209 = EDGE_CURVE ( 'NONE', #13012, #10931, #3888, .T. ) ;
#10210 = ORIENTED_EDGE ( 'NONE', *, *, #8752, .F. ) ;
#10211 = CARTESIAN_POINT ( 'NONE',  ( 0.2182387239031201021, 1.693823289467341286, -3.499999999999995115 ) ) ;
#10212 = PRODUCT ( 'Guide Rail Channel Shoe', 'Guide Rail Channel Shoe', '', ( #931 ) ) ;
#10213 = LINE ( 'NONE', #2257, #11420 ) ;
#10214 = SURFACE_SIDE_STYLE ('',( #1290 ) ) ;
#10215 = CARTESIAN_POINT ( 'NONE',  ( 20.00000000000000000, 37.00000000000000711, 25.00000000000000000 ) ) ;
#10216 = EDGE_LOOP ( 'NONE', ( #8636, #9911, #143, #6010, #9090 ) ) ;
#10217 = CARTESIAN_POINT ( 'NONE',  ( 0.1388410611046112797, 3.710337782248037009, 0.5735064479039858609 ) ) ;
#10218 = ADVANCED_FACE ( 'NONE', ( #1979 ), #12136, .F. ) ;
#10219 = CARTESIAN_POINT ( 'NONE',  ( 3.806834918298608539, 3.031088913245512551, 1.749999999999984679 ) ) ;
#10220 = AXIS2_PLACEMENT_3D ( 'NONE', #13283, #6674, #13437 ) ;
#10221 = CARTESIAN_POINT ( 'NONE',  ( -3.999999999999991118, 2.471529427528112777, -3.386887593711393585 ) ) ;
#10222 = LINE ( 'NONE', #354, #10798 ) ;
#10223 = AXIS2_PLACEMENT_3D ( 'NONE', #7946, #276, #13463 ) ;
#10224 = ORIENTED_EDGE ( 'NONE', *, *, #4059, .F. ) ;
#10225 = DIRECTION ( 'NONE',  ( 0.000000000000000000, 0.000000000000000000, -1.000000000000000000 ) ) ;
#10226 = ORIENTED_EDGE ( 'NONE', *, *, #1270, .F. ) ;
#10227 = VECTOR ( 'NONE', #4913, 1000.000000000000000 ) ;
#10228 = EDGE_CURVE ( 'NONE', #4104, #11502, #8698, .T. ) ;
#10229 = ORIENTED_EDGE ( 'NONE', *, *, #9805, .T. ) ;
#10230 = AXIS2_PLACEMENT_3D ( 'NONE', #6033, #8383, #7061 ) ;
#10231 =( LENGTH_UNIT ( ) NAMED_UNIT ( * ) SI_UNIT ( .MILLI., .METRE. ) );
#10232 = CARTESIAN_POINT ( 'NONE',  ( 4.211140560182201398, 2.431303136016537358, -3.445885042887453231 ) ) ;
#10233 = CARTESIAN_POINT ( 'NONE',  ( -5.000000000000000000, -3.131510016925063589, -4.327949577589330410 ) ) ;
#10234 = AXIS2_PLACEMENT_3D ( 'NONE', #11742, #11512, #5012 ) ;
#10235 = CARTESIAN_POINT ( 'NONE',  ( 108.6817075744280743, 59.57655509336061073, 25.00000000000000000 ) ) ;
#10236 = CARTESIAN_POINT ( 'NONE',  ( 0.1381419387119132147, -1.355287006778748582, 3.499999999999997335 ) ) ;
#10237 = CARTESIAN_POINT ( 'NONE',  ( 125.4817075744280572, 69.57655509336046862, 1.592043197460678939E-14 ) ) ;
#10238 = CARTESIAN_POINT ( 'NONE',  ( 27.30499999999998195, 0.000000000000000000, 0.000000000000000000 ) ) ;
#10239 = ORIENTED_EDGE ( 'NONE', *, *, #3975, .F. ) ;
#10240 = CIRCLE ( 'NONE', #1360, 5.000000000000004441 ) ;
#10241 = CARTESIAN_POINT ( 'NONE',  ( -68.68170757442787533, -83.66032599071911591, 33.00000000000002842 ) ) ;
#10242 = AXIS2_PLACEMENT_3D ( 'NONE', #4012, #11601, #1810 ) ;
#10243 = VERTEX_POINT ( 'NONE', #6488 ) ;
#10244 = EDGE_CURVE ( 'NONE', #1954, #13783, #8765, .T. ) ;
#10245 = CARTESIAN_POINT ( 'NONE',  ( -2.687328764639631551, 3.067272167851298192, -0.05923475698270941336 ) ) ;
#10246 = CARTESIAN_POINT ( 'NONE',  ( 33.99999999999998579, 80.00000000000000000, -23.00000000000000000 ) ) ;
#10247 = VECTOR ( 'NONE', #13003, 999.9999999999998863 ) ;
#10248 = ORIENTED_EDGE ( 'NONE', *, *, #10625, .T. ) ;
#10249 =( REPRESENTATION_RELATIONSHIP ('NONE','NONE', #10295, #8802 ) REPRESENTATION_RELATIONSHIP_WITH_TRANSFORMATION ( #13534 )SHAPE_REPRESENTATION_RELATIONSHIP( ) );
#10250 = CARTESIAN_POINT ( 'NONE',  ( 3.000000000000001332, 4.996003610813205418E-16, 2.400000000000013234 ) ) ;
#10251 = CARTESIAN_POINT ( 'NONE',  ( 1.560000000000005826, -1.732050807568885631, 0.000000000000000000 ) ) ;
#10252 = ORIENTED_EDGE ( 'NONE', *, *, #4847, .F. ) ;
#10253 = DIRECTION ( 'NONE',  ( 0.000000000000000000, 0.000000000000000000, -1.000000000000000000 ) ) ;
#10254 = COLOUR_RGB ( '', 0.40784314, 0.44705882, 0.49803922) ;
#10255 = EDGE_LOOP ( 'NONE', ( #6901, #7090, #8587, #3129, #2233, #3772, #11876, #10403 ) ) ;
#10256 = EDGE_CURVE ( 'NONE', #974, #9330, #1440, .T. ) ;
#10257 = EDGE_CURVE ( 'NONE', #13588, #7727, #13355, .T. ) ;
#10258 = VECTOR ( 'NONE', #14197, 1000.000000000000000 ) ;
#10259 = CARTESIAN_POINT ( 'NONE',  ( -3.200000000000000178, -1.410200760929219011E-16, 1.599999999999990319 ) ) ;
#10260 = DIRECTION ( 'NONE',  ( 0.000000000000000000, 0.000000000000000000, -1.000000000000000000 ) ) ;
#10261 = CARTESIAN_POINT ( 'NONE',  ( 4.124214193018060470, -2.028338413290957210, -3.513185186763553958 ) ) ;
#10262 = DIRECTION ( 'NONE',  ( 0.000000000000000000, 0.000000000000000000, 1.000000000000000000 ) ) ;
#10263 = FILL_AREA_STYLE_COLOUR ( '', #1699 ) ;
#10264 = LINE ( 'NONE', #14461, #9780 ) ;
#10265 = DIRECTION ( 'NONE',  ( 0.000000000000000000, -8.482162385747133845E-47, 1.000000000000000000 ) ) ;
#10266 = ORIENTED_EDGE ( 'NONE', *, *, #1431, .T. ) ;
#10267 = CARTESIAN_POINT ( 'NONE',  ( 59.18121602037099649, 13.58289998256015352, 25.00000000000000000 ) ) ;
#10268 = AXIS2_PLACEMENT_3D ( 'NONE', #6930, #1372, #8248 ) ;
#10269 = ORIENTED_EDGE ( 'NONE', *, *, #11159, .F. ) ;
#10270 = DIRECTION ( 'NONE',  ( 0.000000000000000000, 0.000000000000000000, 1.000000000000000000 ) ) ;
#10271 = DIRECTION ( 'NONE',  ( 0.000000000000000000, 0.000000000000000000, -1.000000000000000000 ) ) ;
#10272 = VERTEX_POINT ( 'NONE', #7653 ) ;
#10273 = CARTESIAN_POINT ( 'NONE',  ( 71.80728622811317052, 38.49793223363091954, -28.00000000000000000 ) ) ;
#10274 = ORIENTED_EDGE ( 'NONE', *, *, #3947, .T. ) ;
#10275 = ORIENTED_EDGE ( 'NONE', *, *, #2392, .T. ) ;
#10276 = CIRCLE ( 'NONE', #10532, 10.00000000000000355 ) ;
#10277 = ADVANCED_FACE ( 'NONE', ( #5474 ), #7031, .T. ) ;
#10278 = VERTEX_POINT ( 'NONE', #932 ) ;
#10279 = AXIS2_PLACEMENT_3D ( 'NONE', #9107, #5882, #10365 ) ;
#10280 = ADVANCED_FACE ( 'NONE', ( #4473 ), #9451, .F. ) ;
#10281 = CARTESIAN_POINT ( 'NONE',  ( 20.00000000000000000, -5.510910596163090344E-15, 25.00000000000000000 ) ) ;
#10282 = FACE_OUTER_BOUND ( 'NONE', #7373, .T. ) ;
#10283 = CARTESIAN_POINT ( 'NONE',  ( 22.00000000000000000, 80.00000000000000000, 25.00000000000000000 ) ) ;
#10284 = DIRECTION ( 'NONE',  ( 1.000000000000000000, 0.000000000000000000, 0.000000000000000000 ) ) ;
#10285 = ORIENTED_EDGE ( 'NONE', *, *, #10089, .F. ) ;
#10286 = DIRECTION ( 'NONE',  ( -0.2425356250363328581, 0.9701425001453318764, 0.000000000000000000 ) ) ;
#10287 = FACE_OUTER_BOUND ( 'NONE', #2292, .T. ) ;
#10288 = CARTESIAN_POINT ( 'NONE',  ( 1.151117775318593766E-15, 3.202582148906732318, 1.452965002680436379 ) ) ;
#10289 = DIRECTION ( 'NONE',  ( 1.000000000000000000, 0.000000000000000000, 0.000000000000000000 ) ) ;
#10290 = B_SPLINE_CURVE_WITH_KNOTS ( 'NONE', 3,
 ( #8509, #5431, #7333, #9746, #11883 ),
 .UNSPECIFIED., .F., .F.,
 ( 4, 1, 4 ),
 ( 0.000000000000000000, 0.002309401076758504923, 0.004618802153517009845 ),
 .UNSPECIFIED. ) ;
#10291 = CARTESIAN_POINT ( 'NONE',  ( -4.211405941597120339, -2.460460478483087243, -3.451298436431144978 ) ) ;
#10292 = VECTOR ( 'NONE', #13749, 999.9999999999998863 ) ;
#10293 = CARTESIAN_POINT ( 'NONE',  ( 0.000000000000000000, 189.5765550933606107, -37.00000000000003553 ) ) ;
#10294 = AXIS2_PLACEMENT_3D ( 'NONE', #10267, #11307, #9022 ) ;
#10295 = SHAPE_REPRESENTATION ( 'BR-599', ( #6154, #11300, #13191, #11782, #6387, #1255, #11074, #7088, #2423, #8500, #3604, #6859, #12967, #801, #6623, #565, #2203, #5460, #4093, #1732, #10842, #12470, #3146, #10608, #8966, #14133, #7797, #1491 ), #4320 ) ;
#10296 = EDGE_CURVE ( 'NONE', #1320, #5390, #12071, .T. ) ;
#10297 = CIRCLE ( 'NONE', #6332, 8.000000000000000000 ) ;
#10298 = ORIENTED_EDGE ( 'NONE', *, *, #312, .F. ) ;
#10299 = VECTOR ( 'NONE', #8746, 1000.000000000000000 ) ;
#10300 = ORIENTED_EDGE ( 'NONE', *, *, #2349, .T. ) ;
#10301 = EDGE_CURVE ( 'NONE', #5025, #8755, #8914, .T. ) ;
#10302 = CARTESIAN_POINT ( 'NONE',  ( 47.05443476855437268, 62.09002498982675888, -25.00000000000000000 ) ) ;
#10303 = EDGE_CURVE ( 'NONE', #7846, #11633, #5538, .T. ) ;
#10304 = CIRCLE ( 'NONE', #12637, 2.500000000000002220 ) ;
#10305 = ORIENTED_EDGE ( 'NONE', *, *, #13636, .T. ) ;
#10306 = DIRECTION ( 'NONE',  ( 1.000000000000000000, 0.000000000000000000, 0.000000000000000000 ) ) ;
#10307 =( GEOMETRIC_REPRESENTATION_CONTEXT ( 3 ) GLOBAL_UNCERTAINTY_ASSIGNED_CONTEXT ( ( #10704 ) ) GLOBAL_UNIT_ASSIGNED_CONTEXT ( ( #2803, #4910, #1616 ) ) REPRESENTATION_CONTEXT ( 'NONE', 'WORKASPACE' ) );
#10308 = AXIS2_PLACEMENT_3D ( 'NONE', #11628, #1380, #12803 ) ;
#10309 = CARTESIAN_POINT ( 'NONE',  ( 4.203833317240883716, 1.627343821129582535, -3.297273115243909203 ) ) ;
#10310 = DIRECTION ( 'NONE',  ( 1.000000000000000000, -2.551526159633733968E-19, -1.987661601597216239E-18 ) ) ;
#10311 = AXIS2_PLACEMENT_3D ( 'NONE', #13709, #3676, #10178 ) ;
#10312 = CARTESIAN_POINT ( 'NONE',  ( 6.800000000000084199, 4.618802153517023612, -1.387778780781445676E-14 ) ) ;
#10313 = CARTESIAN_POINT ( 'NONE',  ( 71.80728622811317052, -17.99808865627607801, 28.00000000000000000 ) ) ;
#10314 = DIRECTION ( 'NONE',  ( 0.6696017473163344835, 0.7427203376715302285, 5.778499435349912740E-17 ) ) ;
#10315 = PLANE ( 'NONE',  #10785 ) ;
#10316 = EDGE_CURVE ( 'NONE', #9280, #2086, #4262, .T. ) ;
#10317 = AXIS2_PLACEMENT_3D ( 'NONE', #14342, #4398, #2193 ) ;
#10318 =( GEOMETRIC_REPRESENTATION_CONTEXT ( 3 ) GLOBAL_UNCERTAINTY_ASSIGNED_CONTEXT ( ( #7332 ) ) GLOBAL_UNIT_ASSIGNED_CONTEXT ( ( #2288, #6885, #10113 ) ) REPRESENTATION_CONTEXT ( 'NONE', 'WORKASPACE' ) );
#10319 = VECTOR ( 'NONE', #3821, 1000.000000000000000 ) ;
#10320 = DIRECTION ( 'NONE',  ( 1.000000000000000000, 1.665334536937734071E-16, 0.000000000000000000 ) ) ;
#10321 = ORIENTED_EDGE ( 'NONE', *, *, #13458, .T. ) ;
#10322 = ORIENTED_EDGE ( 'NONE', *, *, #1007, .T. ) ;
#10323 = ORIENTED_EDGE ( 'NONE', *, *, #5300, .F. ) ;
#10324 = ORIENTED_EDGE ( 'NONE', *, *, #9715, .F. ) ;
#10325 = CARTESIAN_POINT ( 'NONE',  ( 5.599999999999994316, 2.020725942163681399, 3.499999999999996003 ) ) ;
#10326 = LINE ( 'NONE', #3609, #6798 ) ;
#10327 = VECTOR ( 'NONE', #3269, 1000.000000000000000 ) ;
#10328 = STYLED_ITEM ( 'NONE', ( #11226 ), #4561 ) ;
#10329 = VECTOR ( 'NONE', #3945, 1000.000000000000000 ) ;
#10330 = VECTOR ( 'NONE', #11513, 999.9999999999998863 ) ;
#10331 =( LENGTH_UNIT ( ) NAMED_UNIT ( * ) SI_UNIT ( .MILLI., .METRE. ) );
#10332 = VERTEX_POINT ( 'NONE', #7812 ) ;
#10333 = FACE_BOUND ( 'NONE', #9978, .T. ) ;
#10334 = EDGE_CURVE ( 'NONE', #9365, #14055, #14345, .T. ) ;
#10335 = CARTESIAN_POINT ( 'NONE',  ( 20.00000000000000355, 17.00000000000000000, 25.00000000000000000 ) ) ;
#10336 = EDGE_LOOP ( 'NONE', ( #8840, #14073, #9802, #613 ) ) ;
#10337 =( GEOMETRIC_REPRESENTATION_CONTEXT ( 3 ) GLOBAL_UNCERTAINTY_ASSIGNED_CONTEXT ( ( #1488 ) ) GLOBAL_UNIT_ASSIGNED_CONTEXT ( ( #9973, #4215, #968 ) ) REPRESENTATION_CONTEXT ( 'NONE', 'WORKASPACE' ) );
#10338 = CARTESIAN_POINT ( 'NONE',  ( 139.9999999999996874, 189.5765550933606107, 47.99999999999998579 ) ) ;
#10339 = VECTOR ( 'NONE', #818, 1000.000000000000000 ) ;
#10340 = CIRCLE ( 'NONE', #13406, 2.500000000000002220 ) ;
#10341 = EDGE_CURVE ( 'NONE', #4966, #11019, #2617, .T. ) ;
#10342 = CARTESIAN_POINT ( 'NONE',  ( -2.000000000000001776, 3.464101615137757495, 0.000000000000000000 ) ) ;
#10343 = LINE ( 'NONE', #9312, #3134 ) ;
#10344 = CARTESIAN_POINT ( 'NONE',  ( 20.00000000000000355, 30.00000000000000711, -25.00000000000000000 ) ) ;
#10345 = DIRECTION ( 'NONE',  ( 0.000000000000000000, 0.000000000000000000, -1.000000000000000000 ) ) ;
#10346 = CARTESIAN_POINT ( 'NONE',  ( 44.55443476855437268, 62.09002498982675888, -25.00000000000000000 ) ) ;
#10347 = DIRECTION ( 'NONE',  ( -1.000000000000000000, -1.723842398015259277E-15, 0.000000000000000000 ) ) ;
#10348 = AXIS2_PLACEMENT_3D ( 'NONE', #12010, #8839, #1085 ) ;
#10349 = CARTESIAN_POINT ( 'NONE',  ( 0.000000000000000000, -0.8660254037844428154, -1.500000000000001332 ) ) ;
#10350 = ORIENTED_EDGE ( 'NONE', *, *, #4631, .F. ) ;
#10351 = DIRECTION ( 'NONE',  ( 0.000000000000000000, 0.000000000000000000, 1.000000000000000000 ) ) ;
#10352 = EDGE_CURVE ( 'NONE', #12535, #696, #11461, .T. ) ;
#10353 = EDGE_CURVE ( 'NONE', #13190, #10931, #632, .T. ) ;
#10354 = CARTESIAN_POINT ( 'NONE',  ( 4.988724804725785944, -4.618802153517009401, 0.000000000000000000 ) ) ;
#10355 = VERTEX_POINT ( 'NONE', #6990 ) ;
#10356 = DIRECTION ( 'NONE',  ( 0.000000000000000000, 0.000000000000000000, -1.000000000000000000 ) ) ;
#10357 = ORIENTED_EDGE ( 'NONE', *, *, #2136, .T. ) ;
#10358 = DIRECTION ( 'NONE',  ( -1.000000000000000000, 0.000000000000000000, 0.000000000000000000 ) ) ;
#10359 = ORIENTED_EDGE ( 'NONE', *, *, #118, .F. ) ;
#10360 = VECTOR ( 'NONE', #4780, 1000.000000000000114 ) ;
#10361 = VERTEX_POINT ( 'NONE', #6860 ) ;
#10362 = CARTESIAN_POINT ( 'NONE',  ( -3.999999999999996447, 2.309401076758494487, -0.5000000000000004441 ) ) ;
#10363 = CARTESIAN_POINT ( 'NONE',  ( -1.307332176164476278, 48.39629610561008377, 7.789394415675250372 ) ) ;
#10364 = B_SPLINE_CURVE_WITH_KNOTS ( 'NONE', 3,
 ( #10970, #5342, #9804, #12016, #813, #1989 ),
 .UNSPECIFIED., .F., .F.,
 ( 4, 2, 4 ),
 ( 0.002044882221487530176, 0.003063384235218498484, 0.004081886248949466792 ),
 .UNSPECIFIED. ) ;
#10365 = DIRECTION ( 'NONE',  ( -1.000000000000000000, 0.000000000000000000, 0.000000000000000000 ) ) ;
#10366 = AXIS2_PLACEMENT_3D ( 'NONE', #2106, #1893, #10953 ) ;
#10367 = FACE_OUTER_BOUND ( 'NONE', #12957, .T. ) ;
#10368 = ORIENTED_EDGE ( 'NONE', *, *, #2487, .T. ) ;
#10369 = LINE ( 'NONE', #5887, #436 ) ;
#10370 =( NAMED_UNIT ( * ) PLANE_ANGLE_UNIT ( ) SI_UNIT ( $, .RADIAN. ) );
#10371 = CONTEXT_DEPENDENT_SHAPE_REPRESENTATION ( #14211, #6490 ) ;
#10372 = PRESENTATION_LAYER_ASSIGNMENT (  '', '', ( #12250 ) ) ;
#10373 = DIRECTION ( 'NONE',  ( -0.000000000000000000, -8.482162385747133845E-47, 1.000000000000000000 ) ) ;
#10374 = CARTESIAN_POINT ( 'NONE',  ( -3.999999999999991562, 1.700072946616246972, -3.020308295356175066 ) ) ;
#10375 = DIRECTION ( 'NONE',  ( -0.000000000000000000, 1.000000000000000000, -0.000000000000000000 ) ) ;
#10376 = FACE_OUTER_BOUND ( 'NONE', #626, .T. ) ;
#10377 = AXIS2_PLACEMENT_3D ( 'NONE', #3984, #391, #1630 ) ;
#10378 = ORIENTED_EDGE ( 'NONE', *, *, #6373, .T. ) ;
#10379 = ORIENTED_EDGE ( 'NONE', *, *, #1117, .F. ) ;
#10380 = CARTESIAN_POINT ( 'NONE',  ( 19.99999999999999645, 67.00000000000000000, -25.00000000000000000 ) ) ;
#10381 = ORIENTED_EDGE ( 'NONE', *, *, #14154, .F. ) ;
#10382 = VERTEX_POINT ( 'NONE', #69 ) ;
#10383 = ORIENTED_EDGE ( 'NONE', *, *, #10118, .T. ) ;
#10384 = DIRECTION ( 'NONE',  ( 1.000000000000000000, 0.000000000000000000, 0.000000000000000000 ) ) ;
#10385 = DIRECTION ( 'NONE',  ( 0.000000000000000000, 5.551115123125782702E-17, 1.000000000000000000 ) ) ;
#10386 = CARTESIAN_POINT ( 'NONE',  ( -5.253687112945022442, -3.069398100742061875, -4.666238921072260126 ) ) ;
#10387 = FACE_OUTER_BOUND ( 'NONE', #7113, .T. ) ;
#10388 = DIRECTION ( 'NONE',  ( -0.000000000000000000, -0.000000000000000000, -1.000000000000000000 ) ) ;
#10389 = DIRECTION ( 'NONE',  ( 0.6696017473163342615, -0.7427203376715301175, -5.551115123125782702E-17 ) ) ;
#10390 = CARTESIAN_POINT ( 'NONE',  ( 60.00000000000000000, -6.123233995736768255E-16, -23.00000000000000000 ) ) ;
#10391 = CARTESIAN_POINT ( 'NONE',  ( 0.3208286057739703212, -4.433571671609695564, -0.3503314178412707536 ) ) ;
#10392 = EDGE_CURVE ( 'NONE', #12770, #9644, #5737, .T. ) ;
#10393 = EDGE_CURVE ( 'NONE', #12838, #14315, #3761, .T. ) ;
#10394 = DIRECTION ( 'NONE',  ( 0.000000000000000000, 8.482162385747133845E-47, -1.000000000000000000 ) ) ;
#10395 = ORIENTED_EDGE ( 'NONE', *, *, #9360, .F. ) ;
#10396 = ORIENTED_EDGE ( 'NONE', *, *, #13305, .T. ) ;
#10397 = ORIENTED_EDGE ( 'NONE', *, *, #3162, .T. ) ;
#10398 = CARTESIAN_POINT ( 'NONE',  ( 4.988724804725896966, 4.618802153517016507, 1.387778780781445676E-14 ) ) ;
#10399 = CARTESIAN_POINT ( 'NONE',  ( 3.973110223768753002, -0.6864646529411705389, -3.565797985667472414 ) ) ;
#10400 = EDGE_CURVE ( 'NONE', #2316, #8097, #3722, .T. ) ;
#10401 = EDGE_LOOP ( 'NONE', ( #267, #5711, #6219 ) ) ;
#10402 = EDGE_CURVE ( 'NONE', #12541, #13711, #8085, .T. ) ;
#10403 = ORIENTED_EDGE ( 'NONE', *, *, #10470, .T. ) ;
#10404 = DIRECTION ( 'NONE',  ( 1.000000000000000000, -2.551526159633733968E-19, -1.987661601597216239E-18 ) ) ;
#10405 = VERTEX_POINT ( 'NONE', #10156 ) ;
#10406 = CARTESIAN_POINT ( 'NONE',  ( 20.00000000000000355, 50.00000000000000000, -25.00000000000000000 ) ) ;
#10407 = LINE ( 'NONE', #3759, #11706 ) ;
#10408 = CARTESIAN_POINT ( 'NONE',  ( 47.12907851819101523, 71.79144999128007498, 25.00000000000000000 ) ) ;
#10409 = ORIENTED_EDGE ( 'NONE', *, *, #8756, .T. ) ;
#10410 = AXIS2_PLACEMENT_3D ( 'NONE', #690, #8510, #9747 ) ;
#10411 = ADVANCED_FACE ( 'NONE', ( #1442 ), #1519, .F. ) ;
#10412 = DIRECTION ( 'NONE',  ( 0.000000000000000000, 0.000000000000000000, -1.000000000000000000 ) ) ;
#10413 = DIRECTION ( 'NONE',  ( -1.000000000000000000, 0.000000000000000000, 0.000000000000000000 ) ) ;
#10414 = CYLINDRICAL_SURFACE ( 'NONE', #2778, 5.499999999999975131 ) ;
#10415 = DIRECTION ( 'NONE',  ( 1.000000000000000000, 0.000000000000000000, 0.000000000000000000 ) ) ;
#10416 = ORIENTED_EDGE ( 'NONE', *, *, #11256, .T. ) ;
#10417 = FACE_OUTER_BOUND ( 'NONE', #8036, .T. ) ;
#10418 = DIRECTION ( 'NONE',  ( 1.000000000000000000, 0.000000000000000000, 0.000000000000000000 ) ) ;
#10419 = CARTESIAN_POINT ( 'NONE',  ( 33.99999999999998579, 80.00000000000000000, 23.00000000000000000 ) ) ;
#10420 = ORIENTED_EDGE ( 'NONE', *, *, #2284, .T. ) ;
#10421 = CYLINDRICAL_SURFACE ( 'NONE', #10586, 2.749999999999997780 ) ;
#10422 = ORIENTED_EDGE ( 'NONE', *, *, #7179, .F. ) ;
#10423 = CARTESIAN_POINT ( 'NONE',  ( 4.988724804725896966, 4.618802153517016507, 1.387778780781445676E-14 ) ) ;
#10424 = ORIENTED_EDGE ( 'NONE', *, *, #1743, .T. ) ;
#10425 = ORIENTED_EDGE ( 'NONE', *, *, #10201, .F. ) ;
#10426 = CARTESIAN_POINT ( 'NONE',  ( 53.99999999999997868, -1.324077043022348342E-15, -25.00000000000000000 ) ) ;
#10427 = DIRECTION ( 'NONE',  ( 0.000000000000000000, 0.000000000000000000, 1.000000000000000000 ) ) ;
#10428 = EDGE_CURVE ( 'NONE', #6152, #6044, #5831, .T. ) ;
#10429 = ORIENTED_EDGE ( 'NONE', *, *, #14344, .T. ) ;
#10430 = CARTESIAN_POINT ( 'NONE',  ( 108.6817075744280743, 124.5765550933606107, 25.00000000000000000 ) ) ;
#10431 = EDGE_CURVE ( 'NONE', #4731, #13229, #2471, .T. ) ;
#10432 = CARTESIAN_POINT ( 'NONE',  ( 27.75000000000001066, 0.000000000000000000, 2.055000000000000160 ) ) ;
#10433 = DIRECTION ( 'NONE',  ( -0.000000000000000000, 1.000000000000000000, -0.000000000000000000 ) ) ;
#10434 = CARTESIAN_POINT ( 'NONE',  ( 0.02993401039713880149, 3.373851915354617592, 1.156317065392247878 ) ) ;
#10435 = DIRECTION ( 'NONE',  ( 1.000000000000000000, 0.000000000000000000, 0.000000000000000000 ) ) ;
#10436 = CARTESIAN_POINT ( 'NONE',  ( -3.999999999999991562, -0.8382426107201307319, -2.920612530944965979 ) ) ;
#10437 = DIRECTION ( 'NONE',  ( 0.000000000000000000, -8.482162385747133845E-47, 1.000000000000000000 ) ) ;
#10438 = VECTOR ( 'NONE', #14286, 1000.000000000000000 ) ;
#10439 = CYLINDRICAL_SURFACE ( 'NONE', #8830, 2.500000000000002220 ) ;
#10440 = ORIENTED_EDGE ( 'NONE', *, *, #10946, .F. ) ;
#10441 = CARTESIAN_POINT ( 'NONE',  ( 0.000000000000000000, 0.000000000000000000, 1.599999999999990319 ) ) ;
#10442 = ORIENTED_EDGE ( 'NONE', *, *, #3144, .F. ) ;
#10443 = EDGE_CURVE ( 'NONE', #4578, #6602, #13535, .T. ) ;
#10444 = ORIENTED_EDGE ( 'NONE', *, *, #2084, .T. ) ;
#10445 = CARTESIAN_POINT ( 'NONE',  ( 22.00000000000000711, 20.00000000000000355, 25.00000000000000000 ) ) ;
#10446 = EDGE_CURVE ( 'NONE', #5579, #13171, #2533, .T. ) ;
#10447 = CARTESIAN_POINT ( 'NONE',  ( 54.25585977000769589, 23.28432498401347672, -25.00000000000000000 ) ) ;
#10448 = DIRECTION ( 'NONE',  ( -0.000000000000000000, 1.000000000000000000, -0.000000000000000000 ) ) ;
#10449 = APPLICATION_CONTEXT ( 'automotive_design' ) ;
#10450 = CARTESIAN_POINT ( 'NONE',  ( 58.68170757442803165, 39.57655509336063204, 33.00000000000000000 ) ) ;
#10451 = DIRECTION ( 'NONE',  ( 0.000000000000000000, -1.000000000000000000, 0.000000000000000000 ) ) ;
#10452 = AXIS2_PLACEMENT_3D ( 'NONE', #2387, #7796, #13453 ) ;
#10453 = DIRECTION ( 'NONE',  ( 0.000000000000000000, 1.000000000000000000, 0.000000000000000000 ) ) ;
#10454 = DIRECTION ( 'NONE',  ( 8.658726361542619729E-32, -5.046468293750711996E-16, 1.000000000000000000 ) ) ;
#10455 = DIRECTION ( 'NONE',  ( 0.000000000000000000, 0.000000000000000000, 1.000000000000000000 ) ) ;
#10456 = LINE ( 'NONE', #12731, #9612 ) ;
#10457 = EDGE_CURVE ( 'NONE', #12827, #4078, #4480, .T. ) ;
#10458 = PRODUCT_DEFINITION_SHAPE ( 'NONE', 'NONE',  #3656 ) ;
#10459 = EDGE_LOOP ( 'NONE', ( #7592, #12125 ) ) ;
#10460 = CARTESIAN_POINT ( 'NONE',  ( -5.332495919439446207E-15, -3.660093687634839110, -1.660531772554321384 ) ) ;
#10461 = ORIENTED_EDGE ( 'NONE', *, *, #9893, .T. ) ;
#10462 = VECTOR ( 'NONE', #9378, 1000.000000000000000 ) ;
#10463 = AXIS2_PLACEMENT_3D ( 'NONE', #1275, #12188, #13295 ) ;
#10464 = VECTOR ( 'NONE', #11101, 1000.000000000000000 ) ;
#10465 = ORIENTED_EDGE ( 'NONE', *, *, #2932, .F. ) ;
#10466 = ORIENTED_EDGE ( 'NONE', *, *, #4090, .F. ) ;
#10467 = ORIENTED_EDGE ( 'NONE', *, *, #12518, .F. ) ;
#10468 = ADVANCED_FACE ( 'NONE', ( #139 ), #280, .T. ) ;
#10469 = ADVANCED_BREP_SHAPE_REPRESENTATION ( '', ( #11914, #11025 ), #10079 ) ;
#10470 = EDGE_CURVE ( 'NONE', #10731, #562, #9193, .T. ) ;
#10471 = LINE ( 'NONE', #2571, #13234 ) ;
#10472 = CARTESIAN_POINT ( 'NONE',  ( 42.20372226782770753, 81.49287499273339108, -25.00000000000000000 ) ) ;
#10473 = CIRCLE ( 'NONE', #10944, 5.000000000000004441 ) ;
#10474 = VECTOR ( 'NONE', #5787, 1000.000000000000000 ) ;
#10475 = EDGE_LOOP ( 'NONE', ( #2125, #12958, #2015 ) ) ;
#10476 = EDGE_CURVE ( 'NONE', #11372, #8967, #13466, .T. ) ;
#10477 = VECTOR ( 'NONE', #2093, 1000.000000000000000 ) ;
#10478 = DIRECTION ( 'NONE',  ( -8.673617379884692214E-19, 0.8660254037844392627, 0.4999999999999990563 ) ) ;
#10479 = DIRECTION ( 'NONE',  ( -1.000000000000000000, 1.892425610156517368E-16, 0.000000000000000000 ) ) ;
#10480 = VERTEX_POINT ( 'NONE', #5679 ) ;
#10481 = ADVANCED_FACE ( 'NONE', ( #11322 ), #202, .F. ) ;
#10482 = CARTESIAN_POINT ( 'NONE',  ( -68.68170757442807428, 29.57655509336051125, 33.00000000000002842 ) ) ;
#10483 = ORIENTED_EDGE ( 'NONE', *, *, #11485, .F. ) ;
#10484 = EDGE_CURVE ( 'NONE', #7883, #8838, #5032, .T. ) ;
#10485 = CARTESIAN_POINT ( 'NONE',  ( -3.511755186886741154, 2.826662030176364304, -3.297382984111596915 ) ) ;
#10486 = FACE_OUTER_BOUND ( 'NONE', #3265, .T. ) ;
#10487 = CARTESIAN_POINT ( 'NONE',  ( 4.175813232069169878, -2.061359961916378492, -3.570380186727409200 ) ) ;
#10488 = DIRECTION ( 'NONE',  ( 0.000000000000000000, 0.000000000000000000, 1.000000000000000000 ) ) ;
#10489 = SURFACE_STYLE_USAGE ( .BOTH. , #7110 ) ;
#10490 = CARTESIAN_POINT ( 'NONE',  ( 5.170224855064536662, 2.788471980053847332, -4.589066185948671439 ) ) ;
#10491 = LINE ( 'NONE', #1639, #3481 ) ;
#10492 = VERTEX_POINT ( 'NONE', #9496 ) ;
#10493 = FILL_AREA_STYLE_COLOUR ( '', #9127 ) ;
#10494 = B_SPLINE_CURVE_WITH_KNOTS ( 'NONE', 3,
 ( #6006, #4926, #3692, #394, #2588, #7035 ),
 .UNSPECIFIED., .F., .F.,
 ( 4, 2, 4 ),
 ( 0.003058795990767246026, 0.004586520967003294459, 0.006114245943239343326 ),
 .UNSPECIFIED. ) ;
#10495 = ORIENTED_EDGE ( 'NONE', *, *, #5722, .T. ) ;
#10496 = DIRECTION ( 'NONE',  ( 1.000000000000000000, 0.000000000000000000, 0.000000000000000000 ) ) ;
#10497 = CARTESIAN_POINT ( 'NONE',  ( 2.742797192660133998, 3.035247456002194255, -3.133250573521593640 ) ) ;
#10498 = VECTOR ( 'NONE', #2226, 1000.000000000000000 ) ;
#10499 = ORIENTED_EDGE ( 'NONE', *, *, #2573, .F. ) ;
#10500 = CARTESIAN_POINT ( 'NONE',  ( 20.00000000000000355, 40.00000000000000711, 25.00000000000000000 ) ) ;
#10501 = EDGE_CURVE ( 'NONE', #1523, #7848, #10517, .T. ) ;
#10502 = CARTESIAN_POINT ( 'NONE',  ( 4.966167347451144742, 2.723760149934941754, 3.431994069539810344 ) ) ;
#10503 = CONICAL_SURFACE ( 'NONE', #2556, 2.445500000000002672, 0.7853981633974423948 ) ;
#10504 = VERTEX_POINT ( 'NONE', #7136 ) ;
#10505 = FACE_OUTER_BOUND ( 'NONE', #14463, .T. ) ;
#10506 = VERTEX_POINT ( 'NONE', #9420 ) ;
#10507 = LINE ( 'NONE', #14040, #5918 ) ;
#10508 = CARTESIAN_POINT ( 'NONE',  ( -0.2691907178497369713, 48.50000000000000711, 8.000000000000007105 ) ) ;
#10509 = VERTEX_POINT ( 'NONE', #3801 ) ;
#10510 = CARTESIAN_POINT ( 'NONE',  ( 5.013196232911438344, -2.310564645009316909, 4.002015359328495947 ) ) ;
#10511 = VECTOR ( 'NONE', #11923, 1000.000000000000000 ) ;
#10512 = DIRECTION ( 'NONE',  ( 1.000000000000000000, 0.000000000000000000, 0.000000000000000000 ) ) ;
#10513 =( NAMED_UNIT ( * ) SI_UNIT ( $, .STERADIAN. ) SOLID_ANGLE_UNIT ( ) );
#10514 = DIRECTION ( 'NONE',  ( 1.000000000000000000, 1.913084959030911013E-15, 0.000000000000000000 ) ) ;
#10515 = FILL_AREA_STYLE_COLOUR ( '', #8879 ) ;
#10516 = AXIS2_PLACEMENT_3D ( 'NONE', #12507, #10310, #9283 ) ;
#10517 = LINE ( 'NONE', #6198, #4696 ) ;
#10518 = CARTESIAN_POINT ( 'NONE',  ( -3.999999999999991562, 0.8730390046630041034, -2.923132639555956480 ) ) ;
#10519 = PLANE ( 'NONE',  #2164 ) ;
#10520 = DIRECTION ( 'NONE',  ( 1.000000000000000000, 0.000000000000000000, 0.000000000000000000 ) ) ;
#10521 = EDGE_CURVE ( 'NONE', #2985, #13323, #9600, .T. ) ;
#10522 = CONICAL_SURFACE ( 'NONE', #2118, 3.000000000000000888, 0.9599310885968798113 ) ;
#10523 = EDGE_LOOP ( 'NONE', ( #5322, #3672, #2119, #8629, #13261 ) ) ;
#10524 = CARTESIAN_POINT ( 'NONE',  ( -108.6817075744281027, 39.57655509336044730, 33.00000000000002842 ) ) ;
#10525 = ORIENTED_EDGE ( 'NONE', *, *, #1189, .F. ) ;
#10526 = EDGE_LOOP ( 'NONE', ( #1592, #12790, #4381, #6903 ) ) ;
#10527 = CARTESIAN_POINT ( 'NONE',  ( 33.99999999999998579, 80.00000000000000000, -23.00000000000000000 ) ) ;
#10528 = CARTESIAN_POINT ( 'NONE',  ( -1.312671235360381994, -3.860931062424226567, -0.05923475698271308404 ) ) ;
#10529 = CARTESIAN_POINT ( 'NONE',  ( 20.00000000000000711, 20.00000000000000355, -25.00000000000000000 ) ) ;
#10530 = PLANE ( 'NONE',  #1868 ) ;
#10531 = CARTESIAN_POINT ( 'NONE',  ( 20.00000000000000000, -5.510910596163090344E-15, 25.00000000000000000 ) ) ;
#10532 = AXIS2_PLACEMENT_3D ( 'NONE', #13963, #717, #8539 ) ;
#10533 = AXIS2_PLACEMENT_3D ( 'NONE', #2287, #4212, #6597 ) ;
#10534 = DIRECTION ( 'NONE',  ( 1.000000000000000000, 0.000000000000000000, 0.000000000000000000 ) ) ;
#10535 = APPLICATION_PROTOCOL_DEFINITION ( 'draft international standard', 'automotive_design', 1998, #2890 ) ;
#10536 = DIRECTION ( 'NONE',  ( -0.9701425001453319874, -0.2425356250363330801, 0.000000000000000000 ) ) ;
#10537 = AXIS2_PLACEMENT_3D ( 'NONE', #2916, #5499, #12939 ) ;
#10538 = LINE ( 'NONE', #8040, #8904 ) ;
#10539 = EDGE_CURVE ( 'NONE', #7758, #8708, #10669, .T. ) ;
#10540 = ADVANCED_FACE ( 'NONE', ( #8238 ), #11682, .T. ) ;
#10541 = DIRECTION ( 'NONE',  ( 0.000000000000000000, 1.000000000000000000, 0.000000000000000000 ) ) ;
#10542 = VERTEX_POINT ( 'NONE', #3941 ) ;
#10543 = VERTEX_POINT ( 'NONE', #497 ) ;
#10544 = APPLICATION_CONTEXT ( 'automotive_design' ) ;
#10546 = ORIENTED_EDGE ( 'NONE', *, *, #9535, .F. ) ;
#10545 = AXIS2_PLACEMENT_3D ( 'NONE', #5838, #3748, #11414 ) ;
#10547 = CARTESIAN_POINT ( 'NONE',  ( -140.0000000000003411, 189.5765550933606107, -132.0000000000000000 ) ) ;
#10548 = DIRECTION ( 'NONE',  ( -1.000000000000000000, 0.000000000000000000, 0.000000000000000000 ) ) ;
#10549 = AXIS2_PLACEMENT_3D ( 'NONE', #14201, #2867, #13036 ) ;
#10550 = ORIENTED_EDGE ( 'NONE', *, *, #742, .F. ) ;
#10551 = VERTEX_POINT ( 'NONE', #653 ) ;
#10552 = LINE ( 'NONE', #614, #8353 ) ;
#10553 = DIRECTION ( 'NONE',  ( -0.000000000000000000, -0.5000000000000011102, -0.8660254037844379305 ) ) ;
#10554 = EDGE_LOOP ( 'NONE', ( #8119, #6390, #4948, #3119 ) ) ;
#10555 = CARTESIAN_POINT ( 'NONE',  ( 6.250000000000033751, 6.938893903907228378E-15, -1.387778780781445676E-14 ) ) ;
#10556 = ORIENTED_EDGE ( 'NONE', *, *, #13127, .T. ) ;
#10557 = VECTOR ( 'NONE', #5210, 1000.000000000000000 ) ;
#10558 = AXIS2_PLACEMENT_3D ( 'NONE', #3018, #11857, #5114 ) ;
#10559 = DIRECTION ( 'NONE',  ( 0.000000000000000000, 0.000000000000000000, -1.000000000000000000 ) ) ;
#10560 = CARTESIAN_POINT ( 'NONE',  ( 5.103531824934171013, -4.708196996972898063, 1.387778780781445676E-14 ) ) ;
#10561 = DIRECTION ( 'NONE',  ( -1.723842398015259277E-15, 1.000000000000000000, 0.000000000000000000 ) ) ;
#10562 = ORIENTED_EDGE ( 'NONE', *, *, #7451, .T. ) ;
#10563 = CARTESIAN_POINT ( 'NONE',  ( 4.151274195509659926, 4.079825909417491125, -1.343105029898746502E-14 ) ) ;
#10564 = DIRECTION ( 'NONE',  ( 0.000000000000000000, 0.000000000000000000, -1.000000000000000000 ) ) ;
#10565 = ORIENTED_EDGE ( 'NONE', *, *, #14125, .T. ) ;
#10566 = CARTESIAN_POINT ( 'NONE',  ( -0.2117491801717900912, 5.895756138069147667, -4.327903350935046412 ) ) ;
#10567 = CARTESIAN_POINT ( 'NONE',  ( 4.851472949720939454, -1.539600717839007871, -3.999999999999990674 ) ) ;
#10568 = VERTEX_POINT ( 'NONE', #8385 ) ;
#10569 = FILL_AREA_STYLE ('',( #10493 ) ) ;
#10570 = VERTEX_POINT ( 'NONE', #7213 ) ;
#10571 = CARTESIAN_POINT ( 'NONE',  ( 62.10586122665984732, -20.42344490663941414, -35.00000000000000000 ) ) ;
#10572 = AXIS2_PLACEMENT_3D ( 'NONE', #13921, #10833, #7319 ) ;
#10573 = CARTESIAN_POINT ( 'NONE',  ( -0.02511946470933182005, 4.877415451931357282, -3.451298686683612171 ) ) ;
#10574 = EDGE_CURVE ( 'NONE', #13865, #768, #11608, .T. ) ;
#10575 = ORIENTED_EDGE ( 'NONE', *, *, #10341, .T. ) ;
#10576 = CARTESIAN_POINT ( 'NONE',  ( 0.000000000000000000, 0.000000000000000000, 1.599999999999990319 ) ) ;
#10577 = EDGE_CURVE ( 'NONE', #6772, #1377, #8190, .T. ) ;
#10578 = FACE_BOUND ( 'NONE', #13739, .T. ) ;
#10579 = DIRECTION ( 'NONE',  ( 0.000000000000000000, 0.000000000000000000, 1.000000000000000000 ) ) ;
#10580 = VERTEX_POINT ( 'NONE', #6037 ) ;
#10581 = ORIENTED_EDGE ( 'NONE', *, *, #1775, .T. ) ;
#10582 = LINE ( 'NONE', #2688, #11790 ) ;
#10583 = LINE ( 'NONE', #7128, #5195 ) ;
#10584 = ORIENTED_EDGE ( 'NONE', *, *, #5570, .T. ) ;
#10585 = CARTESIAN_POINT ( 'NONE',  ( 5.000000000000001776, 2.886751345948127767, -6.000000000000005329 ) ) ;
#10586 = AXIS2_PLACEMENT_3D ( 'NONE', #13951, #9251, #405 ) ;
#10587 = PRODUCT ( 'hex flange bolt small_iso_ISO 4162 - M5 x 25 x 16-N', 'hex flange bolt small_iso_ISO 4162 - M5 x 25 x 16-N', '', ( #3155 ) ) ;
#10588 = DIRECTION ( 'NONE',  ( 0.000000000000000000, 0.000000000000000000, -1.000000000000000000 ) ) ;
#10589 = VERTEX_POINT ( 'NONE', #10595 ) ;
#10590 = LINE ( 'NONE', #8083, #1607 ) ;
#10591 = EDGE_CURVE ( 'NONE', #2918, #658, #4925, .T. ) ;
#10592 = CARTESIAN_POINT ( 'NONE',  ( 56.68121602037099649, 13.58289998256015352, -25.00000000000000000 ) ) ;
#10593 = EDGE_LOOP ( 'NONE', ( #9431, #5130, #13367, #2972 ) ) ;
#10594 = DIRECTION ( 'NONE',  ( -1.000000000000000000, 0.000000000000000000, 0.000000000000000000 ) ) ;
#10595 = CARTESIAN_POINT ( 'NONE',  ( -4.197393957002300446, -7.772664289393031077E-14, -3.203767560748911780 ) ) ;
#10596 = CARTESIAN_POINT ( 'NONE',  ( 1.560000000000005826, -1.732050807568885631, 0.000000000000000000 ) ) ;
#10597 = DIRECTION ( 'NONE',  ( -1.892425610156516875E-16, -1.000000000000000000, 0.000000000000000000 ) ) ;
#10598 = CARTESIAN_POINT ( 'NONE',  ( 0.000000000000000000, 0.000000000000000000, 0.000000000000000000 ) ) ;
#10599 = VECTOR ( 'NONE', #6511, 1000.000000000000000 ) ;
#10600 = ORIENTED_EDGE ( 'NONE', *, *, #11187, .F. ) ;
#10601 = VERTEX_POINT ( 'NONE', #9340 ) ;
#10602 = CARTESIAN_POINT ( 'NONE',  ( 20.00000000000000000, -5.510910596163090344E-15, 25.00000000000000000 ) ) ;
#10603 = VERTEX_POINT ( 'NONE', #1096 ) ;
#10604 = ORIENTED_EDGE ( 'NONE', *, *, #13756, .F. ) ;
#10605 = CARTESIAN_POINT ( 'NONE',  ( -3.822382184081048351, 49.74063820516850143, 8.000000000000007105 ) ) ;
#10606 = CARTESIAN_POINT ( 'NONE',  ( -1.387778780781445676E-14, -4.618802153517016507, -0.5000000000000004441 ) ) ;
#10607 = CARTESIAN_POINT ( 'NONE',  ( 30.10000000000000497, 29.99999999999999645, -25.00000000000000000 ) ) ;
#10608 = AXIS2_PLACEMENT_3D ( 'NONE', #599, #8322, #10454 ) ;
#10609 = DIRECTION ( 'NONE',  ( 6.608470384673545847E-17, -1.000000000000000000, 0.000000000000000000 ) ) ;
#10610 = ADVANCED_FACE ( 'NONE', ( #7824 ), #728, .T. ) ;
#10611 = DIRECTION ( 'NONE',  ( 0.000000000000000000, 0.000000000000000000, -1.000000000000000000 ) ) ;
#10612 = ORIENTED_EDGE ( 'NONE', *, *, #11418, .F. ) ;
#10613 = PLANE ( 'NONE',  #10549 ) ;
#10614 = CARTESIAN_POINT ( 'NONE',  ( 0.000000000000000000, 0.000000000000000000, -59.50000000000000711 ) ) ;
#10615 = FACE_BOUND ( 'NONE', #12138, .T. ) ;
#10616 = LINE ( 'NONE', #5980, #6809 ) ;
#10617 = AXIS2_PLACEMENT_3D ( 'NONE', #11359, #3414, #1272 ) ;
#10618 = DIRECTION ( 'NONE',  ( 0.000000000000000000, 0.000000000000000000, 1.000000000000000000 ) ) ;
#10619 = EDGE_LOOP ( 'NONE', ( #14218, #1238, #11498, #11443 ) ) ;
#10620 = ADVANCED_FACE ( 'NONE', ( #1945 ), #1316, .F. ) ;
#10621 = ORIENTED_EDGE ( 'NONE', *, *, #4953, .T. ) ;
#10622 = ORIENTED_EDGE ( 'NONE', *, *, #10196, .T. ) ;
#10623 = FACE_BOUND ( 'NONE', #13001, .T. ) ;
#10624 = CARTESIAN_POINT ( 'NONE',  ( 59.10586122665984732, -20.42344490663941414, 23.00000000000000000 ) ) ;
#10625 = EDGE_CURVE ( 'NONE', #3362, #3826, #7482, .T. ) ;
#10626 = EDGE_CURVE ( 'NONE', #14018, #5482, #6431, .T. ) ;
#10627 = ORIENTED_EDGE ( 'NONE', *, *, #12007, .T. ) ;
#10628 = ORIENTED_EDGE ( 'NONE', *, *, #12197, .T. ) ;
#10629 = FACE_OUTER_BOUND ( 'NONE', #4132, .T. ) ;
#10630 = CARTESIAN_POINT ( 'NONE',  ( 4.000000000000003553, 0.000000000000000000, 0.000000000000000000 ) ) ;
#10631 = ORIENTED_EDGE ( 'NONE', *, *, #239, .F. ) ;
#10632 = APPLICATION_CONTEXT ( 'automotive_design' ) ;
#10633 = CARTESIAN_POINT ( 'NONE',  ( 20.00000000000000000, -5.510910596163090344E-15, -25.00000000000000000 ) ) ;
#10634 = ORIENTED_EDGE ( 'NONE', *, *, #4906, .F. ) ;
#10635 = PLANE ( 'NONE',  #6550 ) ;
#10636 = CONICAL_SURFACE ( 'NONE', #360, 4.000000000000000000, 0.8911886515913775009 ) ;
#10637 = DIRECTION ( 'NONE',  ( 0.000000000000000000, 0.000000000000000000, 1.000000000000000000 ) ) ;
#10638 = DIRECTION ( 'NONE',  ( 0.000000000000000000, -8.482162385747133845E-47, 1.000000000000000000 ) ) ;
#10639 = ORIENTED_EDGE ( 'NONE', *, *, #7720, .T. ) ;
#10640 = CARTESIAN_POINT ( 'NONE',  ( 4.175075985190124683, 4.120741555260237554, -6.938893903907228378E-15 ) ) ;
#10641 = CARTESIAN_POINT ( 'NONE',  ( -37.00000000000000711, 29.99999999999999645, 8.000000000000007105 ) ) ;
#10642 =( LENGTH_UNIT ( ) NAMED_UNIT ( * ) SI_UNIT ( .MILLI., .METRE. ) );
#10643 = ORIENTED_EDGE ( 'NONE', *, *, #12899, .T. ) ;
#10644 = CARTESIAN_POINT ( 'NONE',  ( 5.284804376168111162, 3.015249596956805611, -4.666192694417969022 ) ) ;
#10645 = AXIS2_PLACEMENT_3D ( 'NONE', #3627, #395, #8357 ) ;
#10646 = CARTESIAN_POINT ( 'NONE',  ( 62.10586122665987574, -20.42344490663940704, -25.00000000000000000 ) ) ;
#10647 = ORIENTED_EDGE ( 'NONE', *, *, #601, .F. ) ;
#10648 =( NAMED_UNIT ( * ) SI_UNIT ( $, .STERADIAN. ) SOLID_ANGLE_UNIT ( ) );
#10649 = ORIENTED_EDGE ( 'NONE', *, *, #9363, .T. ) ;
#10650 = LINE ( 'NONE', #8366, #5791 ) ;
#10651 = DIRECTION ( 'NONE',  ( -0.9701425001453319874, -0.2425356250363327471, 0.000000000000000000 ) ) ;
#10652 = VERTEX_POINT ( 'NONE', #7751 ) ;
#10653 = CARTESIAN_POINT ( 'NONE',  ( 0.000000000000000000, -4.862606272033103139, -3.445885042887453231 ) ) ;
#10654 = CARTESIAN_POINT ( 'NONE',  ( 4.962664318264674357, 4.324618243609340773, 0.6590959511423351014 ) ) ;
#10655 = CARTESIAN_POINT ( 'NONE',  ( 66.53192852109765454, -5.819950020346492892, 25.00000000000000000 ) ) ;
#10656 = EDGE_LOOP ( 'NONE', ( #11915, #357, #3846, #10600 ) ) ;
#10657 = ORIENTED_EDGE ( 'NONE', *, *, #11056, .T. ) ;
#10658 = DIRECTION ( 'NONE',  ( 0.000000000000000000, 0.000000000000000000, 1.000000000000000000 ) ) ;
#10659 = LINE ( 'NONE', #10803, #1448 ) ;
#10660 = ORIENTED_EDGE ( 'NONE', *, *, #3843, .F. ) ;
#10661 = CARTESIAN_POINT ( 'NONE',  ( 4.086262629614029862, 4.082406995609993317, 0.07093633357110699922 ) ) ;
#10662 = ADVANCED_FACE ( 'NONE', ( #4 ), #4275, .F. ) ;
#10663 = CARTESIAN_POINT ( 'NONE',  ( 5.103531824934115946, 2.354098498486452584, 4.077418205400126894 ) ) ;
#10664 = EDGE_LOOP ( 'NONE', ( #14180, #3730, #6474, #5951 ) ) ;
#10665 = LINE ( 'NONE', #4164, #6959 ) ;
#10666 = DIRECTION ( 'NONE',  ( -1.000000000000000000, 0.000000000000000000, 0.000000000000000000 ) ) ;
#10667 = VERTEX_POINT ( 'NONE', #2130 ) ;
#10668 = FILL_AREA_STYLE ('',( #652 ) ) ;
#10669 = LINE ( 'NONE', #3870, #13829 ) ;
#10670 = CARTESIAN_POINT ( 'NONE',  ( 4.000000000000003553, 0.000000000000000000, 0.000000000000000000 ) ) ;
#10671 = CARTESIAN_POINT ( 'NONE',  ( 3.357433326862117262, -3.835087656846223769, -0.07080520455423312820 ) ) ;
#10672 = EDGE_CURVE ( 'NONE', #658, #10551, #12878, .T. ) ;
#10673 = EDGE_CURVE ( 'NONE', #6239, #11431, #5386, .T. ) ;
#10674 = ORIENTED_EDGE ( 'NONE', *, *, #8702, .T. ) ;
#10675 = DIRECTION ( 'NONE',  ( 1.000000000000000000, 1.665334536937734318E-16, 0.000000000000000000 ) ) ;
#10676 = ORIENTED_EDGE ( 'NONE', *, *, #10443, .F. ) ;
#10677 = CARTESIAN_POINT ( 'NONE',  ( 0.000000000000000000, 0.000000000000000000, -3.699999999999981082 ) ) ;
#10678 = EDGE_CURVE ( 'NONE', #1861, #11793, #6722, .T. ) ;
#10679 = FACE_OUTER_BOUND ( 'NONE', #9850, .T. ) ;
#10680 = CARTESIAN_POINT ( 'NONE',  ( 0.000000000000000000, 48.49999999999999289, 0.000000000000000000 ) ) ;
#10681 = CARTESIAN_POINT ( 'NONE',  ( 21.68170757442799967, 141.2731697022880155, 33.00000000000000000 ) ) ;
#10682 = CARTESIAN_POINT ( 'NONE',  ( 4.755015822784813828, 0.000000000000000000, 0.000000000000000000 ) ) ;
#10683 = APPLICATION_PROTOCOL_DEFINITION ( 'draft international standard', 'automotive_design', 1998, #3827 ) ;
#10684 = CARTESIAN_POINT ( 'NONE',  ( 22.00000000000000000, 60.00000000000000711, 25.00000000000000000 ) ) ;
#10685 = CARTESIAN_POINT ( 'NONE',  ( 3.880206590543183509, -3.396506438958527330, 1.117078279488994630 ) ) ;
#10686 = EDGE_CURVE ( 'NONE', #6772, #14419, #9955, .T. ) ;
#10687 = EDGE_LOOP ( 'NONE', ( #5869, #6060, #14363, #7303 ) ) ;
#10688 = CIRCLE ( 'NONE', #4393, 0.5155456020628804703 ) ;
#10689 = LINE ( 'NONE', #14142, #9878 ) ;
#10690 = EDGE_CURVE ( 'NONE', #5040, #10067, #5867, .T. ) ;
#10691 = ORIENTED_EDGE ( 'NONE', *, *, #9309, .T. ) ;
#10692 = EDGE_LOOP ( 'NONE', ( #4945, #11673, #3952, #2122 ) ) ;
#10693 = AXIS2_PLACEMENT_3D ( 'NONE', #563, #3926, #8525 ) ;
#10694 = DIRECTION ( 'NONE',  ( 0.000000000000000000, 0.000000000000000000, 1.000000000000000000 ) ) ;
#10695 = CARTESIAN_POINT ( 'NONE',  ( -2.100000000000000977, -9.254442493598004305E-17, -4.699999999999981526 ) ) ;
#10696 = ORIENTED_EDGE ( 'NONE', *, *, #13134, .T. ) ;
#10697 = CIRCLE ( 'NONE', #13278, 3.299999999999997158 ) ;
#10698 = CARTESIAN_POINT ( 'NONE',  ( 0.7030283904627421254, -5.367609061415554272, -4.396693167834692773 ) ) ;
#10699 = VECTOR ( 'NONE', #8695, 1000.000000000000114 ) ;
#10700 = CARTESIAN_POINT ( 'NONE',  ( -0.7030283904623975122, -5.367609061414145621, -4.396693167834326843 ) ) ;
#10701 = EDGE_LOOP ( 'NONE', ( #11000, #13941, #3534, #11952 ) ) ;
#10702 = EDGE_CURVE ( 'NONE', #9034, #1523, #1451, .T. ) ;
#10703 = CYLINDRICAL_SURFACE ( 'NONE', #1721, 16.00000000000001421 ) ;
#10704 = UNCERTAINTY_MEASURE_WITH_UNIT (LENGTH_MEASURE( 1.000000000000000082E-05 ), #2803, 'distance_accuracy_value', 'NONE');
#10705 = CYLINDRICAL_SURFACE ( 'NONE', #8426, 2.500000000000002220 ) ;
#10706 = CARTESIAN_POINT ( 'NONE',  ( 129.3408537872138595, 199.5765550933606107, -75.00000000000001421 ) ) ;
#10707 = DIRECTION ( 'NONE',  ( 0.000000000000000000, 0.000000000000000000, 1.000000000000000000 ) ) ;
#10708 = B_SPLINE_CURVE_WITH_KNOTS ( 'NONE', 3,
 ( #10606, #3138, #3956, #8250, #10528, #2708, #13978, #8397 ),
 .UNSPECIFIED., .F., .F.,
 ( 4, 2, 2, 4 ),
 ( 2.465131517300305892E-07, 0.001183067374689865392, 0.001774477805458931972, 0.002365888236227998986 ),
 .UNSPECIFIED. ) ;
#10709 = CIRCLE ( 'NONE', #13996, 5.499999999999976907 ) ;
#10710 = ORIENTED_EDGE ( 'NONE', *, *, #2702, .T. ) ;
#10711 = AXIS2_PLACEMENT_3D ( 'NONE', #9417, #11681, #10666 ) ;
#10712 = CARTESIAN_POINT ( 'NONE',  ( -18.12748877629581656, 43.82334295289051340, 8.000000000000007105 ) ) ;
#10713 = LINE ( 'NONE', #9543, #1626 ) ;
#10714 = ORIENTED_EDGE ( 'NONE', *, *, #1235, .F. ) ;
#10715 = LINE ( 'NONE', #1793, #9743 ) ;
#10716 = CYLINDRICAL_SURFACE ( 'NONE', #979, 2.500000000000002220 ) ;
#10717 = ORIENTED_EDGE ( 'NONE', *, *, #2680, .T. ) ;
#10718 =( LENGTH_UNIT ( ) NAMED_UNIT ( * ) SI_UNIT ( .MILLI., .METRE. ) );
#10719 = EDGE_LOOP ( 'NONE', ( #11693, #9048, #4662, #11820, #4567, #3575, #10996 ) ) ;
#10720 = CARTESIAN_POINT ( 'NONE',  ( 3.973110223767151616, -2.262970274364543210E-11, -3.565797985667430225 ) ) ;
#10721 = CARTESIAN_POINT ( 'NONE',  ( 2.712778981738061201, -3.052578478158764597, -3.130620751971683990 ) ) ;
#10722 = ORIENTED_EDGE ( 'NONE', *, *, #2258, .F. ) ;
#10723 = LINE ( 'NONE', #3055, #3222 ) ;
#10724 = EDGE_CURVE ( 'NONE', #7481, #4363, #1994, .T. ) ;
#10725 = DIRECTION ( 'NONE',  ( -2.273843122241288438E-18, -5.551115123125783935E-17, -1.000000000000000000 ) ) ;
#10726 = EDGE_CURVE ( 'NONE', #1344, #11757, #3168, .T. ) ;
#10727 = ORIENTED_EDGE ( 'NONE', *, *, #7348, .F. ) ;
#10728 = ORIENTED_EDGE ( 'NONE', *, *, #7433, .T. ) ;
#10729 = CARTESIAN_POINT ( 'NONE',  ( -2.449848172108558764, -3.432307619358754724, -3.203702292528892048 ) ) ;
#10730 = CARTESIAN_POINT ( 'NONE',  ( -3.057313426867662720, -4.281874658697580216, -4.357628883416065690 ) ) ;
#10731 = VERTEX_POINT ( 'NONE', #875 ) ;
#10732 = EDGE_CURVE ( 'NONE', #10823, #535, #6501, .T. ) ;
#10733 = CARTESIAN_POINT ( 'NONE',  ( 3.974175853609984710, 3.450041667725513683, -1.156004144283957480 ) ) ;
#10734 = CARTESIAN_POINT ( 'NONE',  ( 5.000000000000001776, 2.886751345948152192, -0.5999999999999894307 ) ) ;
#10735 = SURFACE_STYLE_FILL_AREA ( #2993 ) ;
#10736 = CARTESIAN_POINT ( 'NONE',  ( 3.973110223767151616, -2.262970274364543210E-11, -3.565797985667430225 ) ) ;
#10737 = ORIENTED_EDGE ( 'NONE', *, *, #8010, .F. ) ;
#10738 = DIRECTION ( 'NONE',  ( 0.7071067811865483499, 0.7071067811865467956, 0.000000000000000000 ) ) ;
#10739 = DIRECTION ( 'NONE',  ( 1.000000000000000000, 0.000000000000000000, 0.000000000000000000 ) ) ;
#10740 = AXIS2_PLACEMENT_3D ( 'NONE', #7225, #13979, #12876 ) ;
#10741 = FACE_OUTER_BOUND ( 'NONE', #1313, .T. ) ;
#10742 = EDGE_CURVE ( 'NONE', #9259, #3170, #3100, .T. ) ;
#10743 = ADVANCED_FACE ( 'NONE', ( #11121 ), #14090, .T. ) ;
#10744 = ORIENTED_EDGE ( 'NONE', *, *, #8716, .T. ) ;
#10745 = ORIENTED_EDGE ( 'NONE', *, *, #14097, .T. ) ;
#10746 = AXIS2_PLACEMENT_3D ( 'NONE', #13396, #12281, #2399 ) ;
#10747 = ORIENTED_EDGE ( 'NONE', *, *, #3700, .T. ) ;
#10748 = ORIENTED_EDGE ( 'NONE', *, *, #14246, .T. ) ;
#10749 = CARTESIAN_POINT ( 'NONE',  ( 95.04167153547044222, -149.6197612287760705, 28.00000000000000000 ) ) ;
#10750 = FACE_OUTER_BOUND ( 'NONE', #9349, .T. ) ;
#10751 = PLANE ( 'NONE',  #1159 ) ;
#10752 = CARTESIAN_POINT ( 'NONE',  ( 5.103531824934226080, -2.354098498486466351, -4.077418205400154427 ) ) ;
#10753 = DIRECTION ( 'NONE',  ( 1.000000000000000000, 0.000000000000000000, 0.000000000000000000 ) ) ;
#10754 = APPLICATION_PROTOCOL_DEFINITION ( 'draft international standard', 'automotive_design', 1998, #552 ) ;
#10755 = CARTESIAN_POINT ( 'NONE',  ( 2.804994570502175044, 3.229033611042453344, -3.226374918436819339 ) ) ;
#10756 = ADVANCED_FACE ( 'NONE', ( #8639 ), #11698, .F. ) ;
#10757 = CARTESIAN_POINT ( 'NONE',  ( 64.03192852109765454, -5.819950020346492892, 25.00000000000000000 ) ) ;
#10758 = CIRCLE ( 'NONE', #10268, 3.499999999999999112 ) ;
#10759 = CARTESIAN_POINT ( 'NONE',  ( 0.8665032349992187743, 5.555903485205162085, -4.490643565754959710 ) ) ;
#10760 = EDGE_CURVE ( 'NONE', #3285, #1341, #7596, .T. ) ;
#10761 = ORIENTED_EDGE ( 'NONE', *, *, #13033, .F. ) ;
#10762 = ADVANCED_FACE ( 'NONE', ( #10387 ), #9060, .T. ) ;
#10763 = ORIENTED_EDGE ( 'NONE', *, *, #8091, .F. ) ;
#10764 = ORIENTED_EDGE ( 'NONE', *, *, #13189, .T. ) ;
#10765 = CIRCLE ( 'NONE', #10279, 2.500000000000002220 ) ;
#10766 = DIRECTION ( 'NONE',  ( 1.000000000000000000, 0.000000000000000000, 0.000000000000000000 ) ) ;
#10767 = DIRECTION ( 'NONE',  ( -1.000000000000000000, 0.000000000000000000, 0.000000000000000000 ) ) ;
#10768 =( NAMED_UNIT ( * ) PLANE_ANGLE_UNIT ( ) SI_UNIT ( $, .RADIAN. ) );
#10769 = EDGE_CURVE ( 'NONE', #2847, #6911, #9665, .T. ) ;
#10770 = EDGE_LOOP ( 'NONE', ( #11546, #12343, #7576, #2028 ) ) ;
#10771 = ORIENTED_EDGE ( 'NONE', *, *, #751, .F. ) ;
#10772 = CARTESIAN_POINT ( 'NONE',  ( 21.68170757442799967, 141.2731697022880155, -28.00000000000000000 ) ) ;
#10773 = VECTOR ( 'NONE', #11537, 1000.000000000000114 ) ;
#10774 = VECTOR ( 'NONE', #8443, 1000.000000000000000 ) ;
#10775 = CARTESIAN_POINT ( 'NONE',  ( 4.000000000000002665, 1.941961291383483390, -0.3515519931180288160 ) ) ;
#10776 = ORIENTED_EDGE ( 'NONE', *, *, #12325, .F. ) ;
#10777 = DIRECTION ( 'NONE',  ( -0.000000000000000000, -1.000000000000000000, -0.000000000000000000 ) ) ;
#10778 = VECTOR ( 'NONE', #407, 1000.000000000000000 ) ;
#10779 = ORIENTED_EDGE ( 'NONE', *, *, #13068, .F. ) ;
#10780 = DIRECTION ( 'NONE',  ( 0.000000000000000000, 0.000000000000000000, 1.000000000000000000 ) ) ;
#10781 = CARTESIAN_POINT ( 'NONE',  ( 5.253368672218638125, 3.033033817057769532, -4.659491423763650886 ) ) ;
#10782 = CARTESIAN_POINT ( 'NONE',  ( 39.70372226782770753, 81.49287499273339108, 25.00000000000000000 ) ) ;
#10783 = VERTEX_POINT ( 'NONE', #8178 ) ;
#10784 = CARTESIAN_POINT ( 'NONE',  ( 62.10586122665986863, -20.42344490663937151, -33.00000000000000000 ) ) ;
#10785 = AXIS2_PLACEMENT_3D ( 'NONE', #9211, #6138, #12511 ) ;
#10786 = CARTESIAN_POINT ( 'NONE',  ( 20.00000000000000000, 47.00000000000000000, -25.00000000000000000 ) ) ;
#10787 = EDGE_LOOP ( 'NONE', ( #5836, #1728, #14049, #1822, #1305 ) ) ;
#10788 = EDGE_CURVE ( 'NONE', #6997, #10492, #12572, .T. ) ;
#10789 = CARTESIAN_POINT ( 'NONE',  ( 4.755015822784813828, 0.000000000000000000, 0.000000000000000000 ) ) ;
#10790 = ORIENTED_EDGE ( 'NONE', *, *, #11418, .T. ) ;
#10791 = CARTESIAN_POINT ( 'NONE',  ( 0.4012132626380313649, 5.541862106709766422, -0.4203182062997399826 ) ) ;
#10792 = CARTESIAN_POINT ( 'NONE',  ( 4.988724804725896966, -2.309401076758484272, 4.000000000000003553 ) ) ;
#10793 = ORIENTED_EDGE ( 'NONE', *, *, #11788, .T. ) ;
#10794 = CARTESIAN_POINT ( 'NONE',  ( 60.00000000000000000, -6.123233995736768255E-16, 25.00000000000000000 ) ) ;
#10795 = VECTOR ( 'NONE', #13819, 1000.000000000000000 ) ;
#10796 = CARTESIAN_POINT ( 'NONE',  ( 0.000000000000000000, 0.000000000000000000, 0.000000000000000000 ) ) ;
#10797 = ADVANCED_FACE ( 'NONE', ( #4756 ), #7962, .F. ) ;
#10798 = VECTOR ( 'NONE', #501, 1000.000000000000000 ) ;
#10799 = AXIS2_PLACEMENT_3D ( 'NONE', #697, #7614, #5151 ) ;
#10800 = ORIENTED_EDGE ( 'NONE', *, *, #1606, .T. ) ;
#10801 = ORIENTED_EDGE ( 'NONE', *, *, #13972, .T. ) ;
#10802 = FACE_OUTER_BOUND ( 'NONE', #359, .T. ) ;
#10803 = CARTESIAN_POINT ( 'NONE',  ( 36.99999999999999289, 80.00000000000000000, 25.00000000000000000 ) ) ;
#10804 = ORIENTED_EDGE ( 'NONE', *, *, #6173, .F. ) ;
#10805 = CARTESIAN_POINT ( 'NONE',  ( 5.103279350327357911, -2.353751664345912875, 4.076817471046950025 ) ) ;
#10806 = DIRECTION ( 'NONE',  ( -1.000000000000000000, 2.551526159633733968E-19, 1.987661601597216239E-18 ) ) ;
#10807 = AXIS2_PLACEMENT_3D ( 'NONE', #6610, #8952, #12261 ) ;
#10808 = SURFACE_STYLE_USAGE ( .BOTH. , #7288 ) ;
#10809 = VECTOR ( 'NONE', #6392, 1000.000000000000000 ) ;
#10810 = EDGE_CURVE ( 'NONE', #9280, #1954, #1460, .T. ) ;
#10811 = DIRECTION ( 'NONE',  ( 1.000000000000000000, 0.000000000000000000, 0.000000000000000000 ) ) ;
#10812 = AXIS2_PLACEMENT_3D ( 'NONE', #738, #6361, #12806 ) ;
#10813 = VERTEX_POINT ( 'NONE', #2482 ) ;
#10814 = ADVANCED_FACE ( 'NONE', ( #2637 ), #5752, .F. ) ;
#10815 = DIRECTION ( 'NONE',  ( 0.000000000000000000, 0.000000000000000000, -1.000000000000000000 ) ) ;
#10816 = CARTESIAN_POINT ( 'NONE',  ( 4.086262629614022757, 1.979770830881075305, 3.570936333571099297 ) ) ;
#10817 = VERTEX_POINT ( 'NONE', #8991 ) ;
#10818 = ORIENTED_EDGE ( 'NONE', *, *, #5717, .F. ) ;
#10819 = AXIS2_PLACEMENT_3D ( 'NONE', #11425, #2582, #3684 ) ;
#10820 = VECTOR ( 'NONE', #11049, 1000.000000000000000 ) ;
#10821 = ORIENTED_EDGE ( 'NONE', *, *, #12274, .T. ) ;
#10822 = DIRECTION ( 'NONE',  ( -1.000000000000000000, -3.286707217423839940E-17, -2.273843122241288053E-18 ) ) ;
#10823 = VERTEX_POINT ( 'NONE', #10096 ) ;
#10824 = ORIENTED_EDGE ( 'NONE', *, *, #5101, .F. ) ;
#10825 = DIRECTION ( 'NONE',  ( 0.000000000000000000, 0.000000000000000000, -1.000000000000000000 ) ) ;
#10826 = CARTESIAN_POINT ( 'NONE',  ( 20.00000000000000711, 20.00000000000000355, 25.00000000000000000 ) ) ;
#10827 = DIRECTION ( 'NONE',  ( 0.000000000000000000, 0.000000000000000000, 1.000000000000000000 ) ) ;
#10828 = CARTESIAN_POINT ( 'NONE',  ( -5.000000000000000000, 2.886751345948127767, -6.000000000000005329 ) ) ;
#10829 = DIRECTION ( 'NONE',  ( 0.000000000000000000, 0.000000000000000000, 1.000000000000000000 ) ) ;
#10830 = APPLICATION_PROTOCOL_DEFINITION ( 'draft international standard', 'automotive_design', 1998, #5574 ) ;
#10831 = FACE_OUTER_BOUND ( 'NONE', #5292, .T. ) ;
#10832 = FACE_OUTER_BOUND ( 'NONE', #6328, .T. ) ;
#10833 = DIRECTION ( 'NONE',  ( -1.000000000000000000, 0.000000000000000000, 0.000000000000000000 ) ) ;
#10834 = EDGE_LOOP ( 'NONE', ( #1672, #9985, #5340, #7816 ) ) ;
#10835 = DIRECTION ( 'NONE',  ( 0.000000000000000000, -1.000000000000000000, 0.000000000000000000 ) ) ;
#10836 = PRODUCT_DEFINITION_FORMATION_WITH_SPECIFIED_SOURCE ( 'ANY', '', #8232, .NOT_KNOWN. ) ;
#10837 = CARTESIAN_POINT ( 'NONE',  ( 20.00000000000000355, 40.00000000000000711, -25.00000000000000000 ) ) ;
#10838 =( LENGTH_UNIT ( ) NAMED_UNIT ( * ) SI_UNIT ( .MILLI., .METRE. ) );
#10839 = AXIS2_PLACEMENT_3D ( 'NONE', #3574, #4735, #5799 ) ;
#10840 = EDGE_CURVE ( 'NONE', #3118, #13250, #3597, .T. ) ;
#10841 = ORIENTED_EDGE ( 'NONE', *, *, #4462, .F. ) ;
#10842 = AXIS2_PLACEMENT_3D ( 'NONE', #9209, #5978, #2485 ) ;
#10843 = FACE_OUTER_BOUND ( 'NONE', #12222, .T. ) ;
#10844 = CARTESIAN_POINT ( 'NONE',  ( 4.000000000000003553, 0.1981133338132486654, -4.511085718839590031E-15 ) ) ;
#10845 = DIRECTION ( 'NONE',  ( 0.000000000000000000, 0.000000000000000000, -1.000000000000000000 ) ) ;
#10846 = VECTOR ( 'NONE', #1876, 1000.000000000000000 ) ;
#10847 = EDGE_CURVE ( 'NONE', #11506, #13079, #9285, .T. ) ;
#10848 = UNCERTAINTY_MEASURE_WITH_UNIT (LENGTH_MEASURE( 1.000000000000000082E-05 ), #11208, 'distance_accuracy_value', 'NONE');
#10849 = DIRECTION ( 'NONE',  ( -1.000000000000000000, 0.000000000000000000, 0.000000000000000000 ) ) ;
#10850 = CARTESIAN_POINT ( 'NONE',  ( 22.00000000000000000, 60.00000000000000711, 25.00000000000000000 ) ) ;
#10851 = FACE_OUTER_BOUND ( 'NONE', #12807, .T. ) ;
#10852 = CARTESIAN_POINT ( 'NONE',  ( 62.10586122665984732, -20.42344490663941414, 35.00000000000000000 ) ) ;
#10853 = CARTESIAN_POINT ( 'NONE',  ( 4.755015822784813828, 0.000000000000000000, 0.000000000000000000 ) ) ;
#10854 = DIRECTION ( 'NONE',  ( -1.000000000000000000, -2.312964634635743450E-16, 0.000000000000000000 ) ) ;
#10855 = EDGE_CURVE ( 'NONE', #254, #6531, #7004, .T. ) ;
#10856 = DIRECTION ( 'NONE',  ( 0.000000000000000000, 0.000000000000000000, -1.000000000000000000 ) ) ;
#10857 = ORIENTED_EDGE ( 'NONE', *, *, #10228, .F. ) ;
#10858 = CLOSED_SHELL ( 'NONE', ( #10468, #12445, #3740, #2458, #12108, #1481, #9447, #7884, #6667, #11504, #13114, #4253, #11327, #8194, #6401, #13743, #3350, #7979, #6712, #4729, #12888, #3922, #7613, #9974, #7904, #1911, #13975, #7248, #2279, #11178, #9419, #10540, #1459, #2718, #1218, #6557, #2954, #7968, #2683, #8859, #8511, #8417, #4379, #3441, #4042, #3158, #370, #6119, #6744, #10762, #1576, #5052, #13265, #13593 ) ) ;
#10859 = DIRECTION ( 'NONE',  ( 0.000000000000000000, 0.000000000000000000, 1.000000000000000000 ) ) ;
#10860 =( BOUNDED_SURFACE ( )  B_SPLINE_SURFACE ( 3, 2, ( 
 ( #10661, #11908, #2843 ),
 ( #6191, #9565, #4011 ),
 ( #8458, #6257, #10733 ),
 ( #712, #10937, #4452 ),
 ( #10130, #9921, #8878 ),
 ( #6686, #7564, #12115 ) ),
 .UNSPECIFIED., .F., .F., .T. ) 
 B_SPLINE_SURFACE_WITH_KNOTS ( ( 4, 2, 4 ),
 ( 3, 3 ),
 ( 0.01651999345535504898, 0.01858032176739834312, 0.02064065007944164074 ),
 ( 0.000000000000000000, 1.000000000000000000 ),
 .UNSPECIFIED. ) 
 GEOMETRIC_REPRESENTATION_ITEM ( )  RATIONAL_B_SPLINE_SURFACE ( (
 ( 1.000000000000000000, 0.8047781103519391355, 1.000000000000000000),
 ( 1.000000000000000000, 0.8123785825601861355, 1.000000000000000000),
 ( 1.000000000000000000, 0.8190671539791591904, 1.000000000000000000),
 ( 1.000000000000000000, 0.8192352254831551939, 1.000000000000000000),
 ( 1.000000000000000000, 0.8126129677214093405, 1.000000000000000000),
 ( 1.000000000000000000, 0.8047712537969733404, 1.000000000000000000) ) ) 
 REPRESENTATION_ITEM ( '' )  SURFACE ( )  );
#10861 = CARTESIAN_POINT ( 'NONE',  ( 2.725758460532844207, -3.045084772582480781, -2.920601398289143891 ) ) ;
#10862 = ORIENTED_EDGE ( 'NONE', *, *, #1266, .T. ) ;
#10863 = LINE ( 'NONE', #14173, #3462 ) ;
#10864 = CYLINDRICAL_SURFACE ( 'NONE', #8488, 2.500000000000002220 ) ;
#10865 = EDGE_LOOP ( 'NONE', ( #1001, #3263, #8299, #10550 ) ) ;
#10866 = EDGE_CURVE ( 'NONE', #10163, #10570, #6507, .T. ) ;
#10867 = ORIENTED_EDGE ( 'NONE', *, *, #1962, .F. ) ;
#10868 = LINE ( 'NONE', #839, #1258 ) ;
#10869 = CARTESIAN_POINT ( 'NONE',  ( 95.04167153547044222, -149.6197612287760705, -28.00000000000000000 ) ) ;
#10870 = VERTEX_POINT ( 'NONE', #1376 ) ;
#10871 = CARTESIAN_POINT ( 'NONE',  ( -118.6817075744281595, 69.57655509336025546, 0.000000000000000000 ) ) ;
#10872 = PLANE ( 'NONE',  #3538 ) ;
#10873 = CARTESIAN_POINT ( 'NONE',  ( 53.99999999999997868, -1.347111479062091166E-15, -25.00000000000000000 ) ) ;
#10874 = CARTESIAN_POINT ( 'NONE',  ( 118.6817075744280316, 109.5765550933604828, -3.299999999999976730 ) ) ;
#10875 = ORIENTED_EDGE ( 'NONE', *, *, #9758, .T. ) ;
#10876 = SURFACE_STYLE_FILL_AREA ( #46 ) ;
#10877 = DIRECTION ( 'NONE',  ( 0.000000000000000000, -1.000000000000000000, 0.000000000000000000 ) ) ;
#10878 = LINE ( 'NONE', #8388, #5337 ) ;
#10879 = AXIS2_PLACEMENT_3D ( 'NONE', #6835, #10191, #13722 ) ;
#10880 = VERTEX_POINT ( 'NONE', #5822 ) ;
#10881 = EDGE_CURVE ( 'NONE', #3193, #7235, #5632, .T. ) ;
#10882 = ADVANCED_FACE ( 'NONE', ( #11476 ), #5691, .F. ) ;
#10883 = EDGE_LOOP ( 'NONE', ( #11053, #13160, #3808, #1895 ) ) ;
#10884 = CARTESIAN_POINT ( 'NONE',  ( 42.20372226782770753, 81.49287499273339108, -25.00000000000000000 ) ) ;
#10885 = ORIENTED_EDGE ( 'NONE', *, *, #2359, .F. ) ;
#10886 = DIRECTION ( 'NONE',  ( 0.000000000000000000, 0.000000000000000000, 1.000000000000000000 ) ) ;
#10887 = CARTESIAN_POINT ( 'NONE',  ( 5.236872748402767286, 8.765285303662936917E-14, -4.357689166958464533 ) ) ;
#10888 = B_SPLINE_CURVE_WITH_KNOTS ( 'NONE', 3,
 ( #1528, #6932, #5972, #5748, #9352, #9128 ),
 .UNSPECIFIED., .F., .F.,
 ( 4, 2, 4 ),
 ( 0.002044882221487524538, 0.003063384235218490244, 0.004081886248949456383 ),
 .UNSPECIFIED. ) ;
#10889 = CARTESIAN_POINT ( 'NONE',  ( 1.307332176164478943, 48.39629610561006956, 7.789394415675249483 ) ) ;
#10890 = CARTESIAN_POINT ( 'NONE',  ( 129.3408537872138595, 189.5765550933606107, -9.000000000000007105 ) ) ;
#10891 = CARTESIAN_POINT ( 'NONE',  ( -3.081487911019577365E-30, 3.469446951953614189E-15, -4.900000000000015454 ) ) ;
#10892 = APPLICATION_PROTOCOL_DEFINITION ( 'draft international standard', 'automotive_design', 1998, #6041 ) ;
#10893 = DIRECTION ( 'NONE',  ( 0.000000000000000000, 0.000000000000000000, 1.000000000000000000 ) ) ;
#10894 = DIRECTION ( 'NONE',  ( 1.000000000000000000, 0.000000000000000000, 0.000000000000000000 ) ) ;
#10895 = ORIENTED_EDGE ( 'NONE', *, *, #9790, .F. ) ;
#10896 = FACE_OUTER_BOUND ( 'NONE', #3925, .T. ) ;
#10897 = CARTESIAN_POINT ( 'NONE',  ( 20.00000000000000000, 37.00000000000000711, -25.00000000000000000 ) ) ;
#10898 = AXIS2_PLACEMENT_3D ( 'NONE', #5358, #13433, #3328 ) ;
#10899 = DIRECTION ( 'NONE',  ( 0.000000000000000000, -8.482162385747133845E-47, 1.000000000000000000 ) ) ;
#10900 = CARTESIAN_POINT ( 'NONE',  ( 5.000000000000001776, 1.953108124182678207, -0.2699991669428366547 ) ) ;
#10901 = DIRECTION ( 'NONE',  ( 1.000000000000000000, 0.000000000000000000, 0.000000000000000000 ) ) ;
#10902 = EDGE_CURVE ( 'NONE', #433, #13172, #3665, .T. ) ;
#10903 = SURFACE_STYLE_USAGE ( .BOTH. , #12985 ) ;
#10904 = ORIENTED_EDGE ( 'NONE', *, *, #13277, .T. ) ;
#10905 = PLANE ( 'NONE',  #9762 ) ;
#10906 = CARTESIAN_POINT ( 'NONE',  ( 4.000000000000004441, 0.3987449864459970406, -0.01220643443060221052 ) ) ;
#10907 = FACE_OUTER_BOUND ( 'NONE', #1388, .T. ) ;
#10908 = ORIENTED_EDGE ( 'NONE', *, *, #6598, .F. ) ;
#10909 = AXIS2_PLACEMENT_3D ( 'NONE', #2180, #13302, #4594 ) ;
#10910 = ADVANCED_FACE ( 'NONE', ( #4559 ), #3449, .F. ) ;
#10911 = EDGE_CURVE ( 'NONE', #3032, #13783, #9656, .T. ) ;
#10912 = CARTESIAN_POINT ( 'NONE',  ( -2.756166666307275914, -3.027528586793036602, -2.923144239647422538 ) ) ;
#10913 = CARTESIAN_POINT ( 'NONE',  ( 22.00000000000000355, 50.00000000000000000, 25.00000000000000000 ) ) ;
#10914 = DIRECTION ( 'NONE',  ( 1.000000000000000000, 0.000000000000000000, 0.000000000000000000 ) ) ;
#10915 = FACE_OUTER_BOUND ( 'NONE', #3841, .T. ) ;
#10916 = CARTESIAN_POINT ( 'NONE',  ( 1.560000000000005826, -0.8660254037844428154, -1.500000000000001332 ) ) ;
#10917 = DIRECTION ( 'NONE',  ( 0.000000000000000000, 0.000000000000000000, -1.000000000000000000 ) ) ;
#10918 =( NAMED_UNIT ( * ) PLANE_ANGLE_UNIT ( ) SI_UNIT ( $, .RADIAN. ) );
#10919 = AXIS2_PLACEMENT_3D ( 'NONE', #4318, #14328, #916 ) ;
#10920 = CARTESIAN_POINT ( 'NONE',  ( 0.000000000000000000, 3.000000000000002665, 2.400000000000013234 ) ) ;
#10921 = ORIENTED_EDGE ( 'NONE', *, *, #4220, .F. ) ;
#10922 = DIRECTION ( 'NONE',  ( -1.000000000000000000, 0.000000000000000000, 0.000000000000000000 ) ) ;
#10923 = EDGE_CURVE ( 'NONE', #5260, #9673, #9124, .T. ) ;
#10924 = CARTESIAN_POINT ( 'NONE',  ( 3.455075492488635991, -2.624013387858225244, -3.016622336522302383 ) ) ;
#10925 = ORIENTED_EDGE ( 'NONE', *, *, #4568, .T. ) ;
#10926 = CARTESIAN_POINT ( 'NONE',  ( -4.166666666666666963, 3.367876570272815950, -4.118275046351177693 ) ) ;
#10927 = FACE_BOUND ( 'NONE', #12077, .T. ) ;
#10928 = EDGE_CURVE ( 'NONE', #13561, #13520, #8433, .T. ) ;
#10929 = ADVANCED_FACE ( 'NONE', ( #4972 ), #11784, .F. ) ;
#10930 = CONICAL_SURFACE ( 'NONE', #12340, 4.000000000000004441, 1.047197551196600296 ) ;
#10931 = VERTEX_POINT ( 'NONE', #7444 ) ;
#10932 = CIRCLE ( 'NONE', #4636, 2.500000000000002220 ) ;
#10933 = ORIENTED_EDGE ( 'NONE', *, *, #5871, .F. ) ;
#10934 = DIRECTION ( 'NONE',  ( -0.000000000000000000, -0.5000000000000011102, -0.8660254037844379305 ) ) ;
#10935 = CARTESIAN_POINT ( 'NONE',  ( -3.789464654225616513, 47.54647181849109217, 5.306690203119769578 ) ) ;
#10936 = VERTEX_POINT ( 'NONE', #13034 ) ;
#10937 = CARTESIAN_POINT ( 'NONE',  ( 3.948103430090707189, 2.682758828852394917, -2.353325403974035446 ) ) ;
#10938 = CARTESIAN_POINT ( 'NONE',  ( -3.999999999999996447, 0.3987449864459917670, -0.01220643443059570010 ) ) ;
#10939 = CYLINDRICAL_SURFACE ( 'NONE', #12812, 2.500000000000002220 ) ;
#10940 = SHAPE_REPRESENTATION ( 'High-Tension Retraction Spring', ( #11025 ), #7056 ) ;
#10941 = CARTESIAN_POINT ( 'NONE',  ( -5.170224855064538438, 2.788471980053851773, -4.589066185948671439 ) ) ;
#10942 = EDGE_LOOP ( 'NONE', ( #12448, #8189, #11760, #81 ) ) ;
#10943 = SURFACE_STYLE_FILL_AREA ( #13381 ) ;
#10944 = AXIS2_PLACEMENT_3D ( 'NONE', #9714, #5035, #11990 ) ;
#10945 = DIRECTION ( 'NONE',  ( -0.2425356250363328581, 0.9701425001453318764, 0.000000000000000000 ) ) ;
#10946 = EDGE_CURVE ( 'NONE', #12513, #6374, #5047, .T. ) ;
#10947 = VECTOR ( 'NONE', #10945, 1000.000000000000114 ) ;
#10948 = DIRECTION ( 'NONE',  ( 1.000000000000000000, 1.665334536937734318E-16, 0.000000000000000000 ) ) ;
#10949 = VECTOR ( 'NONE', #3792, 1000.000000000000000 ) ;
#10950 = ORIENTED_EDGE ( 'NONE', *, *, #1429, .F. ) ;
#10951 = EDGE_LOOP ( 'NONE', ( #2884, #11146 ) ) ;
#10952 = ORIENTED_EDGE ( 'NONE', *, *, #107, .F. ) ;
#10953 = DIRECTION ( 'NONE',  ( -1.000000000000000000, 0.000000000000000000, 0.000000000000000000 ) ) ;
#10954 = VERTEX_POINT ( 'NONE', #13982 ) ;
#10955 = AXIS2_PLACEMENT_3D ( 'NONE', #10165, #2126, #13547 ) ;
#10956 = LINE ( 'NONE', #6416, #10511 ) ;
#10957 = LINE ( 'NONE', #1897, #12378 ) ;
#10958 = CARTESIAN_POINT ( 'NONE',  ( 3.999740995676851707, 47.42835276639851116, 4.270072082080261566 ) ) ;
#10959 = DIRECTION ( 'NONE',  ( 0.000000000000000000, 0.000000000000000000, -1.000000000000000000 ) ) ;
#10960 = PLANE ( 'NONE',  #9138 ) ;
#10961 = SHAPE_DEFINITION_REPRESENTATION ( #1224, #10295 ) ;
#10962 = CARTESIAN_POINT ( 'NONE',  ( 20.00000000000000000, 70.00000000000000000, -25.00000000000000000 ) ) ;
#10963 = EDGE_CURVE ( 'NONE', #11964, #9506, #1531, .T. ) ;
#10964 = CARTESIAN_POINT ( 'NONE',  ( 20.00000000000000000, 70.00000000000000000, -25.00000000000000000 ) ) ;
#10965 = AXIS2_PLACEMENT_3D ( 'NONE', #11100, #11320, #5535 ) ;
#10966 = EDGE_LOOP ( 'NONE', ( #7462, #11059, #14247, #8714 ) ) ;
#10967 =( GEOMETRIC_REPRESENTATION_CONTEXT ( 3 ) GLOBAL_UNCERTAINTY_ASSIGNED_CONTEXT ( ( #759 ) ) GLOBAL_UNIT_ASSIGNED_CONTEXT ( ( #7893, #6796, #3519 ) ) REPRESENTATION_CONTEXT ( 'NONE', 'WORKASPACE' ) );
#10968 = DIRECTION ( 'NONE',  ( 1.000000000000000000, 0.000000000000000000, 0.000000000000000000 ) ) ;
#10969 = DIRECTION ( 'NONE',  ( -0.2425356250363328581, 0.9701425001453318764, 0.000000000000000000 ) ) ;
#10970 = CARTESIAN_POINT ( 'NONE',  ( 0.000000000000000000, 3.031088913245536087, -1.750000000000001554 ) ) ;
#10971 = CARTESIAN_POINT ( 'NONE',  ( 0.2484800633750049170, 4.430380094434251959, 0.3263565795980906126 ) ) ;
#10972 = CARTESIAN_POINT ( 'NONE',  ( 4.767554269344631557, 3.063547535898108798, -2.693780016422034684 ) ) ;
#10973 = VECTOR ( 'NONE', #7943, 1000.000000000000000 ) ;
#10974 = LINE ( 'NONE', #14430, #6584 ) ;
#10975 = FILL_AREA_STYLE ('',( #4131 ) ) ;
#10976 = EDGE_CURVE ( 'NONE', #10034, #10067, #668, .T. ) ;
#10977 = VERTEX_POINT ( 'NONE', #4037 ) ;
#10978 = ADVANCED_FACE ( 'NONE', ( #8484 ), #953, .F. ) ;
#10979 = CARTESIAN_POINT ( 'NONE',  ( -0.2117491801717982791, -5.895756138069165431, -4.327903350935056181 ) ) ;
#10980 = CARTESIAN_POINT ( 'NONE',  ( 59.10657227073432551, 3.881474981106830313, -25.00000000000000000 ) ) ;
#10981 = DIRECTION ( 'NONE',  ( -0.000000000000000000, -0.000000000000000000, -1.000000000000000000 ) ) ;
#10982 = AXIS2_PLACEMENT_3D ( 'NONE', #469, #9239, #9313 ) ;
#10983 = CYLINDRICAL_SURFACE ( 'NONE', #6785, 2.500000000000002220 ) ;
#10984 = CARTESIAN_POINT ( 'NONE',  ( 61.68121602037100359, 13.58289998256015352, 25.00000000000000000 ) ) ;
#10985 = DIRECTION ( 'NONE',  ( 0.000000000000000000, 0.000000000000000000, -1.000000000000000000 ) ) ;
#10986 = DIRECTION ( 'NONE',  ( 1.000000000000000000, 0.000000000000000000, 0.000000000000000000 ) ) ;
#10987 = DIRECTION ( 'NONE',  ( 1.000000000000000000, 1.927470528863118802E-16, 0.000000000000000000 ) ) ;
#10988 = DIRECTION ( 'NONE',  ( 1.000000000000000000, 0.000000000000000000, 0.000000000000000000 ) ) ;
#10989 = AXIS2_PLACEMENT_3D ( 'NONE', #4415, #946, #14358 ) ;
#10990 = CARTESIAN_POINT ( 'NONE',  ( 20.00000000000000711, 20.00000000000000355, 25.00000000000000000 ) ) ;
#10991 = ORIENTED_EDGE ( 'NONE', *, *, #8065, .F. ) ;
#10992 = COLOUR_RGB ( '', 0.66274510, 0.83137255, 0.94901961) ;
#10993 = ORIENTED_EDGE ( 'NONE', *, *, #5559, .T. ) ;
#10994 = PLANE ( 'NONE',  #3928 ) ;
#10995 = AXIS2_PLACEMENT_3D ( 'NONE', #1931, #12992, #10849 ) ;
#10996 = ORIENTED_EDGE ( 'NONE', *, *, #13383, .T. ) ;
#10997 = CARTESIAN_POINT ( 'NONE',  ( 30.07694101601105530, 130.0000000000000000, -25.00000000000000000 ) ) ;
#10998 = VECTOR ( 'NONE', #2557, 1000.000000000000000 ) ;
#10999 = FACE_BOUND ( 'NONE', #8494, .T. ) ;
#11000 = ORIENTED_EDGE ( 'NONE', *, *, #4631, .T. ) ;
#11001 = CIRCLE ( 'NONE', #9837, 3.299999999999969624 ) ;
#11002 = VERTEX_POINT ( 'NONE', #7379 ) ;
#11003 = DIRECTION ( 'NONE',  ( -1.892425610156516875E-16, -1.000000000000000000, 0.000000000000000000 ) ) ;
#11004 = CARTESIAN_POINT ( 'NONE',  ( 40.00000000000000711, 80.00000000000000000, -25.00000000000000000 ) ) ;
#11005 = EDGE_CURVE ( 'NONE', #13731, #9976, #11853, .T. ) ;
#11006 = AXIS2_PLACEMENT_3D ( 'NONE', #5920, #4575, #11566 ) ;
#11007 = CARTESIAN_POINT ( 'NONE',  ( 0.3572655899080068309, -2.309401076758678339, -4.000000000000031086 ) ) ;
#11008 = CARTESIAN_POINT ( 'NONE',  ( 20.00000000000000000, 27.00000000000000355, -25.00000000000000000 ) ) ;
#11009 = CARTESIAN_POINT ( 'NONE',  ( 76.68170757442796059, 3.003422806631532356E-13, -199.4258611313499330 ) ) ;
#11010 = LINE ( 'NONE', #7568, #8833 ) ;
#11011 = ORIENTED_EDGE ( 'NONE', *, *, #11374, .F. ) ;
#11012 = CARTESIAN_POINT ( 'NONE',  ( 2.369999999999996998, 0.000000000000000000, 4.750000000000000000 ) ) ;
#11013 = B_SPLINE_CURVE_WITH_KNOTS ( 'NONE', 3,
 ( #6838, #11436, #1413, #13448, #7927, #2450 ),
 .UNSPECIFIED., .F., .F.,
 ( 4, 2, 4 ),
 ( 0.000000000000000000, 0.002383230369971169223, 0.004766460739942338445 ),
 .UNSPECIFIED. ) ;
#11014 = EDGE_CURVE ( 'NONE', #4578, #3893, #11001, .T. ) ;
#11015 = EDGE_CURVE ( 'NONE', #10016, #908, #4895, .T. ) ;
#11016 = LINE ( 'NONE', #3204, #10947 ) ;
#11017 = AXIS2_PLACEMENT_3D ( 'NONE', #8696, #10009, #6637 ) ;
#11018 = CARTESIAN_POINT ( 'NONE',  ( 0.3572655899081733644, 2.309401076758504701, -3.999999999999989786 ) ) ;
#11019 = VERTEX_POINT ( 'NONE', #442 ) ;
#11020 = ORIENTED_EDGE ( 'NONE', *, *, #1117, .T. ) ;
#11021 = ORIENTED_EDGE ( 'NONE', *, *, #8323, .F. ) ;
#11022 = CARTESIAN_POINT ( 'NONE',  ( 0.02944718078426967686, -0.6813962075686338382, -3.499999999999996891 ) ) ;
#11023 =( BOUNDED_SURFACE ( )  B_SPLINE_SURFACE ( 3, 2, ( 
 ( #3246, #4287, #11065 ),
 ( #3176, #3325, #6437 ),
 ( #10912, #7834, #7768 ),
 ( #7684, #5354, #12243 ),
 ( #4354, #13270, #9817 ),
 ( #14293, #4502, #8721 ) ),
 .UNSPECIFIED., .F., .F., .T. ) 
 B_SPLINE_SURFACE_WITH_KNOTS ( ( 4, 2, 4 ),
 ( 3, 3 ),
 ( 0.02023740217035201530, 0.02269762987400599993, 0.02515785757765998457 ),
 ( 0.000000000000000000, 1.000000000000000000 ),
 .UNSPECIFIED. ) 
 GEOMETRIC_REPRESENTATION_ITEM ( )  RATIONAL_B_SPLINE_SURFACE ( (
 ( 1.000000000000000000, 0.8047781539129736927, 1.000000000000000000),
 ( 1.000000000000000000, 0.8123770319057125322, 1.000000000000000000),
 ( 1.000000000000000000, 0.8190663783056868485, 1.000000000000000000),
 ( 1.000000000000000000, 0.8192359702877043404, 1.000000000000000000),
 ( 1.000000000000000000, 0.8126134888419832558, 1.000000000000000000),
 ( 1.000000000000000000, 0.8047712368238106873, 1.000000000000000000) ) ) 
 REPRESENTATION_ITEM ( '' )  SURFACE ( )  );
#11024 = EDGE_CURVE ( 'NONE', #2255, #6304, #3406, .T. ) ;
#11025 = AXIS2_PLACEMENT_3D ( 'NONE', #167, #6524, #5441 ) ;
#11026 = ORIENTED_EDGE ( 'NONE', *, *, #8362, .T. ) ;
#11027 = CARTESIAN_POINT ( 'NONE',  ( 60.00000000000000000, -6.123233995736768255E-16, -25.00000000000000000 ) ) ;
#11028 = VECTOR ( 'NONE', #13651, 1000.000000000000000 ) ;
#11029 = AXIS2_PLACEMENT_3D ( 'NONE', #9616, #5226, #4146 ) ;
#11030 = DIRECTION ( 'NONE',  ( 0.000000000000000000, 1.000000000000000000, 0.000000000000000000 ) ) ;
#11031 = CARTESIAN_POINT ( 'NONE',  ( -28.00000000000000355, 29.99999999999999645, 0.000000000000000000 ) ) ;
#11032 = DIRECTION ( 'NONE',  ( 1.000000000000000000, -2.551526159633733968E-19, -1.987661601597216239E-18 ) ) ;
#11033 = CARTESIAN_POINT ( 'NONE',  ( 4.050823680195248855, 2.400527758044911586, 2.978030508226147344 ) ) ;
#11034 = ITEM_DEFINED_TRANSFORMATION ( 'NONE', 'NONE', #11782,  #11025 ) ;
#11035 = EDGE_CURVE ( 'NONE', #1857, #5669, #8320, .T. ) ;
#11036 = CARTESIAN_POINT ( 'NONE',  ( 4.000000000000003553, -2.309401076758511806, -3.133295621305376422 ) ) ;
#11037 = CARTESIAN_POINT ( 'NONE',  ( 4.175813232069169878, 2.061359961916364725, -3.570380186727395433 ) ) ;
#11038 = EDGE_LOOP ( 'NONE', ( #12544, #12699, #13787, #6866 ) ) ;
#11039 = AXIS2_PLACEMENT_3D ( 'NONE', #5051, #9518, #603 ) ;
#11040 = CARTESIAN_POINT ( 'NONE',  ( 4.988724804725896966, 4.618802153517016507, 1.387778780781445676E-14 ) ) ;
#11041 = CIRCLE ( 'NONE', #1701, 6.532899837730830939 ) ;
#11042 = ORIENTED_EDGE ( 'NONE', *, *, #2030, .F. ) ;
#11043 = ORIENTED_EDGE ( 'NONE', *, *, #6439, .F. ) ;
#11044 = LINE ( 'NONE', #14278, #11325 ) ;
#11045 = ORIENTED_EDGE ( 'NONE', *, *, #14400, .T. ) ;
#11046 = EDGE_CURVE ( 'NONE', #55, #908, #10304, .T. ) ;
#11047 = VERTEX_POINT ( 'NONE', #6877 ) ;
#11048 = SURFACE_STYLE_FILL_AREA ( #1092 ) ;
#11049 = DIRECTION ( 'NONE',  ( -1.000000000000000000, -0.000000000000000000, -0.000000000000000000 ) ) ;
#11050 = SURFACE_STYLE_FILL_AREA ( #10020 ) ;
#11051 = CARTESIAN_POINT ( 'NONE',  ( 2.949999999999994404, 3.306546357697852747E-16, -2.699999999999999289 ) ) ;
#11052 = CIRCLE ( 'NONE', #3588, 2.000000000000001776 ) ;
#11053 = ORIENTED_EDGE ( 'NONE', *, *, #9049, .F. ) ;
#11054 = CARTESIAN_POINT ( 'NONE',  ( 4.769962962079068447, 3.881286623614989661, -1.277414369161378849 ) ) ;
#11055 = CARTESIAN_POINT ( 'NONE',  ( 0.000000000000000000, -4.618802153517030717, -3.133295621305376422 ) ) ;
#11056 = EDGE_CURVE ( 'NONE', #3991, #4075, #1199, .T. ) ;
#11057 = DIRECTION ( 'NONE',  ( -0.000000000000000000, -0.000000000000000000, 1.000000000000000000 ) ) ;
#11058 = ORIENTED_EDGE ( 'NONE', *, *, #7032, .T. ) ;
#11059 = ORIENTED_EDGE ( 'NONE', *, *, #4900, .T. ) ;
#11060 = DIRECTION ( 'NONE',  ( -0.2425356250363329969, 0.9701425001453318764, 9.251858538542973800E-15 ) ) ;
#11061 = LINE ( 'NONE', #14291, #7520 ) ;
#11062 = DIRECTION ( 'NONE',  ( -0.2425356250363330801, 0.9701425001453319874, 0.000000000000000000 ) ) ;
#11063 = CIRCLE ( 'NONE', #787, 2.445500000000002672 ) ;
#11064 = VERTEX_POINT ( 'NONE', #517 ) ;
#11065 = CARTESIAN_POINT ( 'NONE',  ( -4.235887314095728051, -2.417314327725976320, -3.451162025751973061 ) ) ;
#11066 = EDGE_CURVE ( 'NONE', #4711, #5054, #11555, .T. ) ;
#11067 = PRODUCT_RELATED_PRODUCT_CATEGORY ( 'part', '', ( #5648 ) ) ;
#11068 = EDGE_CURVE ( 'NONE', #12928, #8708, #2562, .T. ) ;
#11069 = AXIS2_PLACEMENT_3D ( 'NONE', #6204, #13906, #722 ) ;
#11070 = CARTESIAN_POINT ( 'NONE',  ( 1.560000000000005826, 0.000000000000000000, 1.500000000000001332 ) ) ;
#11071 = CARTESIAN_POINT ( 'NONE',  ( -5.384454397937120440, -2.372863027862376680E-16, -4.184454397937131809 ) ) ;
#11072 = PLANE ( 'NONE',  #157 ) ;
#11073 = CARTESIAN_POINT ( 'NONE',  ( 118.6817075744280316, 69.57655509336046862, 0.000000000000000000 ) ) ;
#11074 = AXIS2_PLACEMENT_3D ( 'NONE', #13482, #5628, #2213 ) ;
#11075 = FACE_OUTER_BOUND ( 'NONE', #7355, .T. ) ;
#11076 = ORIENTED_EDGE ( 'NONE', *, *, #9893, .F. ) ;
#11077 = EDGE_LOOP ( 'NONE', ( #13757, #12603, #2860, #7162 ) ) ;
#11078 = CARTESIAN_POINT ( 'NONE',  ( 71.80728622811317052, -20.42344490663941414, 28.00000000000000000 ) ) ;
#11079 = VECTOR ( 'NONE', #8152, 999.9999999999998863 ) ;
#11080 = ORIENTED_EDGE ( 'NONE', *, *, #8871, .F. ) ;
#11081 = CARTESIAN_POINT ( 'NONE',  ( -5.000000000000000000, 2.886751345948124214, -4.284345921091780696 ) ) ;
#11082 = CARTESIAN_POINT ( 'NONE',  ( 0.000000000000000000, 2.081668171172168513E-14, 4.000000000000003553 ) ) ;
#11083 = EDGE_CURVE ( 'NONE', #13714, #3050, #3666, .T. ) ;
#11084 = ORIENTED_EDGE ( 'NONE', *, *, #13988, .F. ) ;
#11085 = LINE ( 'NONE', #6684, #8737 ) ;
#11086 = CARTESIAN_POINT ( 'NONE',  ( -108.6817075744283869, 189.5765550933606107, 33.00000000000002842 ) ) ;
#11087 = DIRECTION ( 'NONE',  ( 0.000000000000000000, 0.000000000000000000, 1.000000000000000000 ) ) ;
#11088 = CARTESIAN_POINT ( 'NONE',  ( 62.10586122665984732, -20.42344490663941414, -35.00000000000000000 ) ) ;
#11089 = CARTESIAN_POINT ( 'NONE',  ( 13.00000000000000355, 24.50000000000001421, 8.000000000000007105 ) ) ;
#11090 = CARTESIAN_POINT ( 'NONE',  ( 3.958491816110948580, 1.406739583088900236, 3.499999999999992450 ) ) ;
#11091 = ORIENTED_EDGE ( 'NONE', *, *, #206, .F. ) ;
#11092 = CARTESIAN_POINT ( 'NONE',  ( 58.68170757442803165, 39.57655509336063204, -33.00000000000000000 ) ) ;
#11093 = CARTESIAN_POINT ( 'NONE',  ( -1.532072935877364915E-15, -6.066067634115591467, -4.659491423763650886 ) ) ;
#11094 = ORIENTED_EDGE ( 'NONE', *, *, #499, .T. ) ;
#11095 = EDGE_CURVE ( 'NONE', #8757, #10405, #6855, .T. ) ;
#11096 = CARTESIAN_POINT ( 'NONE',  ( 0.2175679805369797049, -1.691499766289379147, -3.499999999999996891 ) ) ;
#11097 = ORIENTED_EDGE ( 'NONE', *, *, #5284, .T. ) ;
#11098 = FACE_OUTER_BOUND ( 'NONE', #10593, .T. ) ;
#11099 = DIRECTION ( 'NONE',  ( -0.000000000000000000, -1.000000000000000000, 0.000000000000000000 ) ) ;
#11100 = CARTESIAN_POINT ( 'NONE',  ( 44.62907851819101523, 71.79144999128007498, 25.00000000000000000 ) ) ;
#11101 = DIRECTION ( 'NONE',  ( -1.000000000000000000, 0.000000000000000000, 0.000000000000000000 ) ) ;
#11102 = EDGE_LOOP ( 'NONE', ( #555, #9815, #12172, #11020, #7889 ) ) ;
#11103 = FACE_OUTER_BOUND ( 'NONE', #9579, .T. ) ;
#11104 = ITEM_DEFINED_TRANSFORMATION ( 'NONE', 'NONE', #801,  #11025 ) ;
#11105 = ADVANCED_FACE ( 'NONE', ( #9287, #5977 ), #2484, .F. ) ;
#11106 = AXIS2_PLACEMENT_3D ( 'NONE', #9992, #14460, #4453 ) ;
#11107 = DIRECTION ( 'NONE',  ( 1.000000000000000000, 0.000000000000000000, 0.000000000000000000 ) ) ;
#11108 = DIRECTION ( 'NONE',  ( -1.000000000000000000, 2.551526159633733968E-19, 1.987661601597216239E-18 ) ) ;
#11109 = ORIENTED_EDGE ( 'NONE', *, *, #13950, .F. ) ;
#11110 = EDGE_CURVE ( 'NONE', #8749, #12541, #12890, .T. ) ;
#11111 = DIRECTION ( 'NONE',  ( 0.000000000000000000, 0.000000000000000000, 1.000000000000000000 ) ) ;
#11112 = EDGE_LOOP ( 'NONE', ( #2730, #112 ) ) ;
#11113 = ADVANCED_FACE ( 'NONE', ( #4689 ), #298, .F. ) ;
#11114 = FACE_OUTER_BOUND ( 'NONE', #4251, .T. ) ;
#11115 = ORIENTED_EDGE ( 'NONE', *, *, #5541, .T. ) ;
#11116 = AXIS2_PLACEMENT_3D ( 'NONE', #14157, #14227, #1259 ) ;
#11117 = EDGE_LOOP ( 'NONE', ( #1769, #11169, #1097, #256 ) ) ;
#11118 = CARTESIAN_POINT ( 'NONE',  ( 54.35294117647056567, -1.411764705882362358, -23.00000000000000000 ) ) ;
#11119 = CARTESIAN_POINT ( 'NONE',  ( -5.000000000000000888, 2.424500739214329403, -0.4207179063848094369 ) ) ;
#11120 = CARTESIAN_POINT ( 'NONE',  ( 5.000000000000000888, 0.000000000000000000, 0.000000000000000000 ) ) ;
#11121 = FACE_OUTER_BOUND ( 'NONE', #4817, .T. ) ;
#11122 = ORIENTED_EDGE ( 'NONE', *, *, #1696, .T. ) ;
#11123 = CARTESIAN_POINT ( 'NONE',  ( 71.80728622811317052, -17.99808865627607801, -28.00000000000000000 ) ) ;
#11124 = DIRECTION ( 'NONE',  ( 0.000000000000000000, 0.000000000000000000, 1.000000000000000000 ) ) ;
#11125 = DIRECTION ( 'NONE',  ( 0.000000000000000000, 0.000000000000000000, -1.000000000000000000 ) ) ;
#11126 = CARTESIAN_POINT ( 'NONE',  ( 20.00000000000000355, 17.00000000000000000, -25.00000000000000000 ) ) ;
#11127 = EDGE_LOOP ( 'NONE', ( #3973, #3208, #5162, #12774 ) ) ;
#11128 = CARTESIAN_POINT ( 'NONE',  ( 118.6817075744280316, 109.5765550933604828, 3.299999999999983391 ) ) ;
#11129 = EDGE_CURVE ( 'NONE', #4092, #2047, #3215, .T. ) ;
#11130 = DIRECTION ( 'NONE',  ( -1.000000000000000000, 0.000000000000000000, 0.000000000000000000 ) ) ;
#11131 = DIRECTION ( 'NONE',  ( -0.7071067811865467956, 0.7071067811865483499, -0.000000000000000000 ) ) ;
#11132 = ORIENTED_EDGE ( 'NONE', *, *, #5481, .F. ) ;
#11133 = FACE_OUTER_BOUND ( 'NONE', #7695, .T. ) ;
#11134 = PRODUCT_DEFINITION_CONTEXT ( 'detailed design', #7823, 'design' ) ;
#11135 = CARTESIAN_POINT ( 'NONE',  ( 28.00000000000000355, 29.99999999999999645, -24.99999999999999289 ) ) ;
#11136 = DIRECTION ( 'NONE',  ( 0.000000000000000000, 0.000000000000000000, 1.000000000000000000 ) ) ;
#11137 = CARTESIAN_POINT ( 'NONE',  ( 4.050536630291698970, -2.401306687817075680, 2.976670123173713822 ) ) ;
#11138 = CARTESIAN_POINT ( 'NONE',  ( 5.000882498481339589, 2.309401076758504701, 4.000000000000031086 ) ) ;
#11139 = ORIENTED_EDGE ( 'NONE', *, *, #6153, .T. ) ;
#11140 = CIRCLE ( 'NONE', #9977, 2.500000000000002220 ) ;
#11141 = ORIENTED_EDGE ( 'NONE', *, *, #13972, .F. ) ;
#11142 = CARTESIAN_POINT ( 'NONE',  ( 3.806834918298619641, -3.031088913245550298, -1.750000000000016653 ) ) ;
#11143 = EDGE_CURVE ( 'NONE', #11793, #7871, #9132, .T. ) ;
#11144 = SURFACE_STYLE_USAGE ( .BOTH. , #8803 ) ;
#11145 = CARTESIAN_POINT ( 'NONE',  ( 0.3126073911696169993, -4.041451884327377009, 0.000000000000000000 ) ) ;
#11146 = ORIENTED_EDGE ( 'NONE', *, *, #4337, .T. ) ;
#11147 = ORIENTED_EDGE ( 'NONE', *, *, #10672, .F. ) ;
#11148 = LINE ( 'NONE', #7922, #12704 ) ;
#11149 = CARTESIAN_POINT ( 'NONE',  ( -118.6817075744281595, 69.57655509336025546, -3.299999999999983391 ) ) ;
#11150 = CIRCLE ( 'NONE', #13500, 5.499999999999976907 ) ;
#11151 = DIRECTION ( 'NONE',  ( -1.000000000000000000, 0.000000000000000000, 0.000000000000000000 ) ) ;
#11152 = DIRECTION ( 'NONE',  ( 1.000000000000000000, 3.286707217423839940E-17, 2.273843122241288053E-18 ) ) ;
#11153 = DIRECTION ( 'NONE',  ( 0.000000000000000000, 0.000000000000000000, -1.000000000000000000 ) ) ;
#11154 = CARTESIAN_POINT ( 'NONE',  ( -3.417629563437020401, 3.800333343455476687, -4.019399823475544586 ) ) ;
#11155 = ORIENTED_EDGE ( 'NONE', *, *, #72, .T. ) ;
#11156 = ORIENTED_EDGE ( 'NONE', *, *, #14256, .T. ) ;
#11157 = DIRECTION ( 'NONE',  ( 0.000000000000000000, 1.000000000000000000, -0.000000000000000000 ) ) ;
#11158 = EDGE_CURVE ( 'NONE', #13026, #4341, #6055, .T. ) ;
#11159 = EDGE_CURVE ( 'NONE', #13731, #4830, #8255, .T. ) ;
#11160 = LINE ( 'NONE', #2249, #3681 ) ;
#11161 = AXIS2_PLACEMENT_3D ( 'NONE', #12319, #3256, #4510 ) ;
#11162 = AXIS2_PLACEMENT_3D ( 'NONE', #12865, #12953, #14257 ) ;
#11163 = VERTEX_POINT ( 'NONE', #2714 ) ;
#11164 = VERTEX_POINT ( 'NONE', #4973 ) ;
#11165 = ADVANCED_FACE ( 'NONE', ( #1602 ), #34, .T. ) ;
#11166 = ADVANCED_BREP_SHAPE_REPRESENTATION ( '', ( #6873, #11025 ), #1200 ) ;
#11167 = ORIENTED_EDGE ( 'NONE', *, *, #8195, .F. ) ;
#11168 = CARTESIAN_POINT ( 'NONE',  ( 5.000000000000001776, 2.886751345948152192, -0.5999999999999894307 ) ) ;
#11169 = ORIENTED_EDGE ( 'NONE', *, *, #8635, .T. ) ;
#11170 = CARTESIAN_POINT ( 'NONE',  ( 62.10586122665984732, -20.42344490663941414, -25.00000000000000000 ) ) ;
#11171 = FACE_OUTER_BOUND ( 'NONE', #5017, .T. ) ;
#11172 = DIRECTION ( 'NONE',  ( 0.2425356250363327471, -0.9701425001453319874, -0.000000000000000000 ) ) ;
#11173 = LINE ( 'NONE', #1153, #2760 ) ;
#11174 = VECTOR ( 'NONE', #14185, 1000.000000000000000 ) ;
#11175 = CARTESIAN_POINT ( 'NONE',  ( 21.68170757442808849, 141.2731697022877313, 35.00000000000000000 ) ) ;
#11176 = DIRECTION ( 'NONE',  ( 0.000000000000000000, 0.000000000000000000, 1.000000000000000000 ) ) ;
#11177 = CARTESIAN_POINT ( 'NONE',  ( 61.60657227073433262, 3.881474981106830313, 25.00000000000000000 ) ) ;
#11178 = ADVANCED_FACE ( 'NONE', ( #13916 ), #5826, .T. ) ;
#11179 = CARTESIAN_POINT ( 'NONE',  ( 4.104070371397483541, -2.023683613428362005, 3.505122836902491379 ) ) ;
#11180 = ORIENTED_EDGE ( 'NONE', *, *, #14256, .F. ) ;
#11181 = ORIENTED_EDGE ( 'NONE', *, *, #6820, .T. ) ;
#11182 = AXIS2_PLACEMENT_3D ( 'NONE', #1239, #1164, #7749 ) ;
#11183 = CARTESIAN_POINT ( 'NONE',  ( 4.000000000000003553, -1.942223658245632700, -0.3516579909967693096 ) ) ;
#11184 = ORIENTED_EDGE ( 'NONE', *, *, #6368, .F. ) ;
#11185 = CARTESIAN_POINT ( 'NONE',  ( -5.000000000000000000, 2.886751345948124214, -0.5999999999999894307 ) ) ;
#11186 = FACE_OUTER_BOUND ( 'NONE', #2461, .T. ) ;
#11187 = EDGE_CURVE ( 'NONE', #14055, #10783, #3093, .T. ) ;
#11188 = CARTESIAN_POINT ( 'NONE',  ( 0.03421028094653577600, 3.855830693249152397, 1.321505333908953750 ) ) ;
#11189 = VERTEX_POINT ( 'NONE', #1461 ) ;
#11190 = DIRECTION ( 'NONE',  ( -1.000000000000000000, 0.000000000000000000, 0.000000000000000000 ) ) ;
#11191 = CARTESIAN_POINT ( 'NONE',  ( 27.75000000000001066, 2.789133085058096608E-16, -2.055000000000000160 ) ) ;
#11192 = CARTESIAN_POINT ( 'NONE',  ( 0.000000000000000000, 0.000000000000000000, 0.000000000000000000 ) ) ;
#11193 = FACE_OUTER_BOUND ( 'NONE', #4529, .T. ) ;
#11194 = ORIENTED_EDGE ( 'NONE', *, *, #6140, .T. ) ;
#11195 = B_SPLINE_CURVE_WITH_KNOTS ( 'NONE', 3,
 ( #2875, #1766, #6217, #8559 ),
 .UNSPECIFIED., .F., .F.,
 ( 4, 4 ),
 ( 2.380737582602404047E-07, 0.002336974151641542548 ),
 .UNSPECIFIED. ) ;
#11196 = EDGE_CURVE ( 'NONE', #11484, #12547, #1378, .T. ) ;
#11197 = EDGE_CURVE ( 'NONE', #5916, #11584, #3086, .T. ) ;
#11198 = ORIENTED_EDGE ( 'NONE', *, *, #5819, .F. ) ;
#11199 = CARTESIAN_POINT ( 'NONE',  ( 1.069120652742303742E-15, 4.736522675502173207, -3.381124513963619904 ) ) ;
#11200 = DIRECTION ( 'NONE',  ( 0.000000000000000000, 0.000000000000000000, -1.000000000000000000 ) ) ;
#11201 = VECTOR ( 'NONE', #9353, 1000.000000000000000 ) ;
#11202 = VERTEX_POINT ( 'NONE', #5329 ) ;
#11203 = CARTESIAN_POINT ( 'NONE',  ( 46.97979101891770171, 52.38859998837343568, -25.00000000000000000 ) ) ;
#11204 = DIRECTION ( 'NONE',  ( 1.000000000000000000, 8.619211990076297369E-16, 0.000000000000000000 ) ) ;
#11205 = DIRECTION ( 'NONE',  ( -0.000000000000000000, -0.000000000000000000, -1.000000000000000000 ) ) ;
#11206 = EDGE_CURVE ( 'NONE', #3642, #14419, #6280, .T. ) ;
#11207 = CARTESIAN_POINT ( 'NONE',  ( 20.00000000000000000, 47.00000000000000000, 25.00000000000000000 ) ) ;
#11208 =( LENGTH_UNIT ( ) NAMED_UNIT ( * ) SI_UNIT ( .MILLI., .METRE. ) );
#11209 = CARTESIAN_POINT ( 'NONE',  ( 5.102759246810695259, 2.353060785250063347, 4.075620833351001338 ) ) ;
#11210 = ORIENTED_EDGE ( 'NONE', *, *, #2503, .T. ) ;
#11211 = ORIENTED_EDGE ( 'NONE', *, *, #13248, .T. ) ;
#11212 = LINE ( 'NONE', #8201, #6716 ) ;
#11213 = PRESENTATION_STYLE_ASSIGNMENT (( #11144 ) ) ;
#11214 = AXIS2_PLACEMENT_3D ( 'NONE', #10445, #1596, #2707 ) ;
#11215 = ORIENTED_EDGE ( 'NONE', *, *, #5769, .T. ) ;
#11216 = LINE ( 'NONE', #2438, #4749 ) ;
#11217 = VERTEX_POINT ( 'NONE', #9657 ) ;
#11218 = B_SPLINE_CURVE_WITH_KNOTS ( 'NONE', 3,
 ( #13784, #1265, #2366, #12665 ),
 .UNSPECIFIED., .F., .F.,
 ( 4, 4 ),
 ( 0.000000000000000000, 0.002452478801916370670 ),
 .UNSPECIFIED. ) ;
#11219 = CARTESIAN_POINT ( 'NONE',  ( 129.3408537872138595, 189.5765550933606107, -13.99999999999999645 ) ) ;
#11220 = CARTESIAN_POINT ( 'NONE',  ( -4.817183509279845843, -3.279805190042321517, -4.566911319714218820 ) ) ;
#11221 = ADVANCED_FACE ( 'NONE', ( #12882 ), #1683, .F. ) ;
#11222 = DIRECTION ( 'NONE',  ( -1.000000000000000000, 0.000000000000000000, 0.000000000000000000 ) ) ;
#11223 = STYLED_ITEM ( 'NONE', ( #7426 ), #11635 ) ;
#11224 = CARTESIAN_POINT ( 'NONE',  ( -68.68170757442808849, 39.57655509336051836, -106.9999999999999858 ) ) ;
#11225 = CIRCLE ( 'NONE', #3295, 5.315148208181398104 ) ;
#11226 = PRESENTATION_STYLE_ASSIGNMENT (( #12532 ) ) ;
#11227 = PLANE ( 'NONE',  #13766 ) ;
#11228 = CARTESIAN_POINT ( 'NONE',  ( 61.60657227073433262, 3.881474981106830313, -25.00000000000000000 ) ) ;
#11229 = ORIENTED_EDGE ( 'NONE', *, *, #8145, .F. ) ;
#11230 = CARTESIAN_POINT ( 'NONE',  ( 7.500000000000029310, 29.99999999999999289, 8.000000000000007105 ) ) ;
#11231 = ORIENTED_EDGE ( 'NONE', *, *, #11613, .F. ) ;
#11232 = CARTESIAN_POINT ( 'NONE',  ( -118.6817075744283727, 189.5765550933606107, 33.00000000000002842 ) ) ;
#11233 = B_SPLINE_CURVE_WITH_KNOTS ( 'NONE', 3,
 ( #10663, #1741, #8157, #4807 ),
 .UNSPECIFIED., .F., .F.,
 ( 4, 4 ),
 ( 0.000000000000000000, 0.002376763279741535111 ),
 .UNSPECIFIED. ) ;
#11234 = DIRECTION ( 'NONE',  ( -0.000000000000000000, 1.000000000000000000, -0.000000000000000000 ) ) ;
#11235 = VECTOR ( 'NONE', #13126, 1000.000000000000000 ) ;
#11236 = ORIENTED_EDGE ( 'NONE', *, *, #1307, .F. ) ;
#11237 = VERTEX_POINT ( 'NONE', #14136 ) ;
#11238 = CIRCLE ( 'NONE', #8863, 0.5671001622691687061 ) ;
#11239 = ORIENTED_EDGE ( 'NONE', *, *, #5350, .T. ) ;
#11240 = CARTESIAN_POINT ( 'NONE',  ( 4.960798468790029503, -2.741591971433240627, -3.400875223032410855 ) ) ;
#11241 = EDGE_CURVE ( 'NONE', #14098, #9561, #1912, .T. ) ;
#11242 = ORIENTED_EDGE ( 'NONE', *, *, #4438, .F. ) ;
#11243 = CARTESIAN_POINT ( 'NONE',  ( 8.000000000000000000, 40.49999999999999289, 0.000000000000000000 ) ) ;
#11244 = PRODUCT_DEFINITION ( 'UNKNOWN', '', #3836, #4288 ) ;
#11245 = EDGE_CURVE ( 'NONE', #8967, #7349, #5400, .T. ) ;
#11246 = CARTESIAN_POINT ( 'NONE',  ( 5.236973757159531395, -1.063254885194027333, -4.359289623603279651 ) ) ;
#11247 = DIRECTION ( 'NONE',  ( 0.000000000000000000, 5.551115123125782702E-17, 1.000000000000000000 ) ) ;
#11248 = AXIS2_PLACEMENT_3D ( 'NONE', #6134, #12800, #4119 ) ;
#11249 = CARTESIAN_POINT ( 'NONE',  ( 76.68170757442804586, 59.57655509336061073, 25.00000000000000000 ) ) ;
#11250 =( GEOMETRIC_REPRESENTATION_CONTEXT ( 3 ) GLOBAL_UNCERTAINTY_ASSIGNED_CONTEXT ( ( #621 ) ) GLOBAL_UNIT_ASSIGNED_CONTEXT ( ( #3972, #7094, #2576 ) ) REPRESENTATION_CONTEXT ( 'NONE', 'WORKASPACE' ) );
#11251 = ORIENTED_EDGE ( 'NONE', *, *, #7316, .T. ) ;
#11252 = DIRECTION ( 'NONE',  ( -0.2425356250363328581, 0.9701425001453318764, 0.000000000000000000 ) ) ;
#11253 = ITEM_DEFINED_TRANSFORMATION ( 'NONE', 'NONE', #565,  #11025 ) ;
#11254 = CARTESIAN_POINT ( 'NONE',  ( 0.000000000000000000, 0.000000000000000000, -117.0000000000000000 ) ) ;
#11255 = CARTESIAN_POINT ( 'NONE',  ( 5.024612689793150899, -4.625309484956541262, -2.775557561562891351E-14 ) ) ;
#11256 = EDGE_CURVE ( 'NONE', #13670, #9930, #4183, .T. ) ;
#11257 = B_SPLINE_CURVE_WITH_KNOTS ( 'NONE', 3,
 ( #3721, #10288, #10434, #10217, #279, #4745 ),
 .UNSPECIFIED., .F., .F.,
 ( 4, 2, 4 ),
 ( 0.002044882221487521069, 0.003063384235218490244, 0.004081886248949459853 ),
 .UNSPECIFIED. ) ;
#11258 = FACE_BOUND ( 'NONE', #12276, .T. ) ;
#11259 = ORIENTED_EDGE ( 'NONE', *, *, #10201, .T. ) ;
#11260 = CIRCLE ( 'NONE', #13848, 3.000000000000003553 ) ;
#11261 = DIRECTION ( 'NONE',  ( -0.5000000000000042188, 1.060575238724903710E-16, -0.8660254037844361541 ) ) ;
#11262 = ORIENTED_EDGE ( 'NONE', *, *, #7016, .F. ) ;
#11263 = ORIENTED_EDGE ( 'NONE', *, *, #571, .F. ) ;
#11264 = CARTESIAN_POINT ( 'NONE',  ( -140.0000000000003411, 199.5765550933606107, 47.99999999999998579 ) ) ;
#11265 = DIRECTION ( 'NONE',  ( -1.000000000000000000, -0.000000000000000000, -0.000000000000000000 ) ) ;
#11266 = CARTESIAN_POINT ( 'NONE',  ( 40.00000000000000711, 80.00000000000000000, 25.00000000000000000 ) ) ;
#11267 = DIRECTION ( 'NONE',  ( 0.000000000000000000, 0.000000000000000000, -1.000000000000000000 ) ) ;
#11268 = VERTEX_POINT ( 'NONE', #7228 ) ;
#11269 = DIRECTION ( 'NONE',  ( -3.469446951953692767E-18, 0.5000000000000018874, 0.8660254037844375974 ) ) ;
#11270 = LINE ( 'NONE', #2275, #13384 ) ;
#11271 = CARTESIAN_POINT ( 'NONE',  ( 0.000000000000000000, 0.000000000000000000, 0.000000000000000000 ) ) ;
#11272 = CARTESIAN_POINT ( 'NONE',  ( 21.68170757442799967, 141.2731697022880155, 33.00000000000000000 ) ) ;
#11273 = VERTEX_POINT ( 'NONE', #11703 ) ;
#11274 = VECTOR ( 'NONE', #5696, 1000.000000000000000 ) ;
#11275 = PRODUCT ( 'hex flange bolt small_iso_ISO 4162 - M6 x 25 x 25-C', 'hex flange bolt small_iso_ISO 4162 - M6 x 25 x 25-C', '', ( #5266 ) ) ;
#11276 = EDGE_LOOP ( 'NONE', ( #9456, #4440, #8504, #12940 ) ) ;
#11277 = CARTESIAN_POINT ( 'NONE',  ( -68.68170757442787533, -83.66032599071911591, -117.0000000000000000 ) ) ;
#11278 = CARTESIAN_POINT ( 'NONE',  ( 20.00000000000000000, 70.00000000000000000, 25.00000000000000000 ) ) ;
#11279 = ORIENTED_EDGE ( 'NONE', *, *, #8811, .T. ) ;
#11280 = ORIENTED_EDGE ( 'NONE', *, *, #6778, .T. ) ;
#11281 =( GEOMETRIC_REPRESENTATION_CONTEXT ( 3 ) GLOBAL_UNCERTAINTY_ASSIGNED_CONTEXT ( ( #1628 ) ) GLOBAL_UNIT_ASSIGNED_CONTEXT ( ( #6520, #1049, #8655 ) ) REPRESENTATION_CONTEXT ( 'NONE', 'WORKASPACE' ) );
#11282 = CIRCLE ( 'NONE', #7532, 3.299999999999969624 ) ;
#11283 = EDGE_CURVE ( 'NONE', #904, #144, #507, .T. ) ;
#11284 = LINE ( 'NONE', #12165, #9950 ) ;
#11285 = DIRECTION ( 'NONE',  ( -1.000000000000000000, 0.000000000000000000, 0.000000000000000000 ) ) ;
#11286 = LINE ( 'NONE', #1600, #6045 ) ;
#11287 = DIRECTION ( 'NONE',  ( 0.000000000000000000, 0.000000000000000000, -1.000000000000000000 ) ) ;
#11288 = ORIENTED_EDGE ( 'NONE', *, *, #6865, .T. ) ;
#11289 = APPLICATION_CONTEXT ( 'automotive_design' ) ;
#11290 = VECTOR ( 'NONE', #10260, 1000.000000000000000 ) ;
#11291 = DIRECTION ( 'NONE',  ( 0.000000000000000000, 0.000000000000000000, -1.000000000000000000 ) ) ;
#11292 = AXIS2_PLACEMENT_3D ( 'NONE', #10555, #4844, #5997 ) ;
#11293 = ORIENTED_EDGE ( 'NONE', *, *, #194, .F. ) ;
#11294 = ADVANCED_FACE ( 'NONE', ( #1977 ), #10613, .F. ) ;
#11295 = DIRECTION ( 'NONE',  ( -1.000000000000000000, 2.551526159633733968E-19, 1.987661601597216239E-18 ) ) ;
#11296 = ORIENTED_EDGE ( 'NONE', *, *, #8411, .F. ) ;
#11297 = EDGE_CURVE ( 'NONE', #1344, #2782, #731, .T. ) ;
#11298 = DIRECTION ( 'NONE',  ( -1.000000000000000000, 0.000000000000000000, 1.387778780781446415E-16 ) ) ;
#11299 = CARTESIAN_POINT ( 'NONE',  ( 71.80728622811317052, -20.42344490663941414, -28.00000000000000000 ) ) ;
#11300 = AXIS2_PLACEMENT_3D ( 'NONE', #9133, #8924, #10099 ) ;
#11301 = PLANE ( 'NONE',  #6784 ) ;
#11302 = FACE_OUTER_BOUND ( 'NONE', #9858, .T. ) ;
#11303 = SURFACE_SIDE_STYLE ('',( #13446 ) ) ;
#11304 = CARTESIAN_POINT ( 'NONE',  ( 0.000000000000000000, -4.618802153517030717, -3.133295621305376422 ) ) ;
#11305 = CARTESIAN_POINT ( 'NONE',  ( 4.071447262713911996, 2.020725942163681399, 3.499999999999996003 ) ) ;
#11306 = VERTEX_POINT ( 'NONE', #13108 ) ;
#11307 = DIRECTION ( 'NONE',  ( -0.000000000000000000, -0.000000000000000000, -1.000000000000000000 ) ) ;
#11308 = AXIS2_PLACEMENT_3D ( 'NONE', #3427, #13603, #7802 ) ;
#11309 = ORIENTED_EDGE ( 'NONE', *, *, #1696, .F. ) ;
#11310 = CARTESIAN_POINT ( 'NONE',  ( 0.000000000000000000, 0.000000000000000000, 1.599999999999990319 ) ) ;
#11311 = CYLINDRICAL_SURFACE ( 'NONE', #2747, 3.299999999999976730 ) ;
#11312 = ORIENTED_EDGE ( 'NONE', *, *, #4677, .F. ) ;
#11313 = EDGE_CURVE ( 'NONE', #375, #3412, #7275, .T. ) ;
#11314 = VERTEX_POINT ( 'NONE', #13984 ) ;
#11315 = EDGE_LOOP ( 'NONE', ( #1993, #10017 ) ) ;
#11316 = CARTESIAN_POINT ( 'NONE',  ( 25.90000000000000213, 29.99999999999999645, -25.00000000000000000 ) ) ;
#11317 = ORIENTED_EDGE ( 'NONE', *, *, #12586, .F. ) ;
#11318 = DIRECTION ( 'NONE',  ( 0.5000000000000014433, 0.8660254037844378194, 0.000000000000000000 ) ) ;
#11319 = FACE_OUTER_BOUND ( 'NONE', #5419, .T. ) ;
#11320 = DIRECTION ( 'NONE',  ( 0.000000000000000000, 0.000000000000000000, -1.000000000000000000 ) ) ;
#11321 = PLANE ( 'NONE',  #1127 ) ;
#11322 = FACE_OUTER_BOUND ( 'NONE', #10401, .T. ) ;
#11323 = CARTESIAN_POINT ( 'NONE',  ( 0.2484800633750003651, 2.497823135841271913, -3.673643420401906390 ) ) ;
#11324 = CARTESIAN_POINT ( 'NONE',  ( -118.6817075744279606, -30.42344490663958112, 33.00000000000002842 ) ) ;
#11325 = VECTOR ( 'NONE', #809, 1000.000000000000000 ) ;
#11326 =( BOUNDED_SURFACE ( )  B_SPLINE_SURFACE ( 3, 2, ( 
 ( #7587, #4264, #12072 ),
 ( #2870, #1763, #6215 ),
 ( #10685, #673, #13246 ),
 ( #2329, #8908, #933 ),
 ( #7736, #7813, #12430 ),
 ( #4610, #5680, #4548 ) ),
 .UNSPECIFIED., .F., .F., .T. ) 
 B_SPLINE_SURFACE_WITH_KNOTS ( ( 4, 2, 4 ),
 ( 3, 3 ),
 ( 0.01651999345535503858, 0.01858032176739833966, 0.02064065007944164074 ),
 ( 0.000000000000000000, 1.000000000000000000 ),
 .UNSPECIFIED. ) 
 GEOMETRIC_REPRESENTATION_ITEM ( )  RATIONAL_B_SPLINE_SURFACE ( (
 ( 1.000000000000000000, 0.8047781103519388024, 1.000000000000000000),
 ( 1.000000000000000000, 0.8123785825604552535, 1.000000000000000000),
 ( 1.000000000000000000, 0.8190671539788006994, 1.000000000000000000),
 ( 1.000000000000000000, 0.8192352254835123526, 1.000000000000000000),
 ( 1.000000000000000000, 0.8126129677211405555, 1.000000000000000000),
 ( 1.000000000000000000, 0.8047712537969740065, 1.000000000000000000) ) ) 
 REPRESENTATION_ITEM ( '' )  SURFACE ( )  );
#11327 = ADVANCED_FACE ( 'NONE', ( #4038 ), #7445, .T. ) ;
#11328 = EDGE_CURVE ( 'NONE', #2806, #7329, #8485, .T. ) ;
#11329 = EDGE_LOOP ( 'NONE', ( #14011, #14039, #9000, #431 ) ) ;
#11330 = LINE ( 'NONE', #1300, #8015 ) ;
#11331 = ORIENTED_EDGE ( 'NONE', *, *, #8793, .F. ) ;
#11332 = DIRECTION ( 'NONE',  ( -1.000000000000000000, 0.000000000000000000, 0.000000000000000000 ) ) ;
#11333 = CARTESIAN_POINT ( 'NONE',  ( 5.000000000000001776, 2.886751345948120662, -4.284345921091780696 ) ) ;
#11334 = CARTESIAN_POINT ( 'NONE',  ( 5.599999999999994316, -2.020725942163681399, -3.500000000000010214 ) ) ;
#11335 = CARTESIAN_POINT ( 'NONE',  ( 4.000000000000003553, -2.309401076758511806, -0.5000000000000004441 ) ) ;
#11336 = ORIENTED_EDGE ( 'NONE', *, *, #1387, .T. ) ;
#11337 = CARTESIAN_POINT ( 'NONE',  ( 0.000000000000000000, 0.000000000000000000, 1.159999999999994369 ) ) ;
#11338 = LINE ( 'NONE', #9064, #7023 ) ;
#11339 = ORIENTED_EDGE ( 'NONE', *, *, #13810, .F. ) ;
#11340 = ORIENTED_EDGE ( 'NONE', *, *, #12442, .T. ) ;
#11341 = EDGE_CURVE ( 'NONE', #4128, #6195, #5190, .T. ) ;
#11342 = ADVANCED_FACE ( 'NONE', ( #7513 ), #7310, .F. ) ;
#11343 = CARTESIAN_POINT ( 'NONE',  ( 54.33050351964436686, 32.98574998546678927, 25.00000000000000000 ) ) ;
#11344 = CIRCLE ( 'NONE', #5505, 16.00000000000001421 ) ;
#11345 = EDGE_LOOP ( 'NONE', ( #13398, #2551, #1428, #4917, #10604 ) ) ;
#11346 = B_SPLINE_CURVE_WITH_KNOTS ( 'NONE', 3,
 ( #9702, #8589, #13077, #4303, #6396, #2014 ),
 .UNSPECIFIED., .F., .F.,
 ( 4, 2, 4 ),
 ( 0.000000000000000000, 0.0002514304509865737929, 0.0005028609019731475858 ),
 .UNSPECIFIED. ) ;
#11347 = CARTESIAN_POINT ( 'NONE',  ( 4.686019787951623883, 3.464101615137754386, -1.999999999999987566 ) ) ;
#11348 = CYLINDRICAL_SURFACE ( 'NONE', #11006, 8.000000000000000000 ) ;
#11349 = ORIENTED_EDGE ( 'NONE', *, *, #4614, .T. ) ;
#11350 = ORIENTED_EDGE ( 'NONE', *, *, #11730, .F. ) ;
#11351 = CARTESIAN_POINT ( 'NONE',  ( 21.68170757442806362, 141.2731697022877029, -28.00000000000000000 ) ) ;
#11352 = ADVANCED_FACE ( 'NONE', ( #11785 ), #5265, .T. ) ;
#11353 = CARTESIAN_POINT ( 'NONE',  ( 2.500000000000000444, 3.469446951953614189E-15, -6.000000000000005329 ) ) ;
#11354 = ADVANCED_FACE ( 'NONE', ( #6213 ), #13608, .F. ) ;
#11355 = ORIENTED_EDGE ( 'NONE', *, *, #13922, .T. ) ;
#11356 = DIRECTION ( 'NONE',  ( 1.000000000000000000, 0.000000000000000000, 0.000000000000000000 ) ) ;
#11357 = ADVANCED_FACE ( 'NONE', ( #11103 ), #10960, .F. ) ;
#11358 = VERTEX_POINT ( 'NONE', #3290 ) ;
#11359 = CARTESIAN_POINT ( 'NONE',  ( 88.22284556172391490, 39.57655509336063915, -117.0000000000000000 ) ) ;
#11360 = CARTESIAN_POINT ( 'NONE',  ( 4.960471971868334329, -2.742478347466599686, 3.399327657648741674 ) ) ;
#11361 = CARTESIAN_POINT ( 'NONE',  ( 4.093692494532781723, -2.021783646005765878, -3.501831996793843160 ) ) ;
#11362 = DIRECTION ( 'NONE',  ( -2.273843122241288438E-18, -5.551115123125783935E-17, -1.000000000000000000 ) ) ;
#11363 = CIRCLE ( 'NONE', #12771, 2.500000000000002220 ) ;
#11364 = DIRECTION ( 'NONE',  ( -0.000000000000000000, -0.000000000000000000, -1.000000000000000000 ) ) ;
#11365 = ADVANCED_FACE ( 'NONE', ( #12134 ), #5922, .F. ) ;
#11366 = CARTESIAN_POINT ( 'NONE',  ( 53.99999999999997868, -1.084202172485504434E-15, 25.00000000000000000 ) ) ;
#11367 = ORIENTED_EDGE ( 'NONE', *, *, #8347, .F. ) ;
#11368 = CARTESIAN_POINT ( 'NONE',  ( -8.000000000000000000, 25.49999999999996803, 0.000000000000000000 ) ) ;
#11369 = ORIENTED_EDGE ( 'NONE', *, *, #8052, .F. ) ;
#11370 = CARTESIAN_POINT ( 'NONE',  ( -3.999999999999996447, -3.469446951953614189E-15, 0.000000000000000000 ) ) ;
#11371 = ADVANCED_FACE ( 'NONE', ( #8764 ), #5403, .F. ) ;
#11372 = VERTEX_POINT ( 'NONE', #5473 ) ;
#11373 = DIRECTION ( 'NONE',  ( 0.000000000000000000, 0.000000000000000000, 1.000000000000000000 ) ) ;
#11374 = EDGE_CURVE ( 'NONE', #3835, #8314, #13243, .T. ) ;
#11375 = ORIENTED_EDGE ( 'NONE', *, *, #14183, .F. ) ;
#11376 = VECTOR ( 'NONE', #2981, 1000.000000000000000 ) ;
#11377 = ORIENTED_EDGE ( 'NONE', *, *, #6645, .T. ) ;
#11378 = CARTESIAN_POINT ( 'NONE',  ( 5.103531824934171013, -4.708196996972898063, 1.387778780781445676E-14 ) ) ;
#11379 = EDGE_LOOP ( 'NONE', ( #13220, #8843 ) ) ;
#11380 = DIRECTION ( 'NONE',  ( -0.8660254037844378194, 0.5000000000000014433, -0.000000000000000000 ) ) ;
#11381 = PRODUCT_DEFINITION_SHAPE ( 'NONE', 'NONE',  #4990 ) ;
#11382 = CARTESIAN_POINT ( 'NONE',  ( 5.244723105119098783, 2.047144756275687705, -4.475729968417853755 ) ) ;
#11383 = EDGE_CURVE ( 'NONE', #8027, #13659, #1229, .T. ) ;
#11384 = CARTESIAN_POINT ( 'NONE',  ( 0.000000000000000000, -20.42344490663941414, 33.00000000000000000 ) ) ;
#11385 = EDGE_CURVE ( 'NONE', #10783, #79, #10081, .T. ) ;
#11386 = LINE ( 'NONE', #349, #11632 ) ;
#11387 = CARTESIAN_POINT ( 'NONE',  ( 24.99999999999999289, -4.898587196589414604E-15, -25.00000000000000000 ) ) ;
#11388 = CARTESIAN_POINT ( 'NONE',  ( 2.069940739436584298, -4.578421848776007330, -2.075823643836113210E-14 ) ) ;
#11389 = AXIS2_PLACEMENT_3D ( 'NONE', #12538, #7473, #1724 ) ;
#11390 = DIRECTION ( 'NONE',  ( 0.000000000000000000, 0.000000000000000000, 1.000000000000000000 ) ) ;
#11391 = DIRECTION ( 'NONE',  ( 0.000000000000000000, 4.440892098500620738E-16, 1.000000000000000000 ) ) ;
#11392 = VECTOR ( 'NONE', #14340, 1000.000000000000000 ) ;
#11393 = ORIENTED_EDGE ( 'NONE', *, *, #4843, .F. ) ;
#11394 = ORIENTED_EDGE ( 'NONE', *, *, #10946, .T. ) ;
#11395 = CARTESIAN_POINT ( 'NONE',  ( 28.00000000000000355, 29.99999999999999645, -6.999999999999992006 ) ) ;
#11396 = AXIS2_PLACEMENT_3D ( 'NONE', #536, #9675, #3900 ) ;
#11397 = VECTOR ( 'NONE', #6687, 1000.000000000000000 ) ;
#11398 = ORIENTED_EDGE ( 'NONE', *, *, #13931, .T. ) ;
#11399 = AXIS2_PLACEMENT_3D ( 'NONE', #11766, #10514, #3940 ) ;
#11400 = DIRECTION ( 'NONE',  ( 0.000000000000000000, 0.000000000000000000, 1.000000000000000000 ) ) ;
#11401 = CARTESIAN_POINT ( 'NONE',  ( 5.185163620697179176, 2.993655612200650573, -4.630826434870604302 ) ) ;
#11402 = DIRECTION ( 'NONE',  ( -1.000000000000000000, -0.000000000000000000, -0.000000000000000000 ) ) ;
#11403 = EDGE_CURVE ( 'NONE', #992, #1210, #2151, .T. ) ;
#11404 = CARTESIAN_POINT ( 'NONE',  ( -108.6817075744279748, -20.42344490663957046, 33.00000000000002842 ) ) ;
#11405 = EDGE_LOOP ( 'NONE', ( #9021, #7657, #9504, #680 ) ) ;
#11406 = DIRECTION ( 'NONE',  ( 0.000000000000000000, 5.551115123125782702E-17, 1.000000000000000000 ) ) ;
#11407 =( BOUNDED_SURFACE ( )  B_SPLINE_SURFACE ( 3, 2, ( 
 ( #7628, #3270, #5584 ),
 ( #12050, #2091, #13376 ),
 ( #10057, #3136, #1063 ),
 ( #2021, #909, #2304 ),
 ( #4376, #6753, #6462 ),
 ( #40, #8813, #7710 ) ),
 .UNSPECIFIED., .F., .F., .T. ) 
 B_SPLINE_SURFACE_WITH_KNOTS ( ( 4, 2, 4 ),
 ( 3, 3 ),
 ( 0.01651999345535506980, 0.01858032176739836394, 0.02064065007944165808 ),
 ( 0.000000000000000000, 1.000000000000000000 ),
 .UNSPECIFIED. ) 
 GEOMETRIC_REPRESENTATION_ITEM ( )  RATIONAL_B_SPLINE_SURFACE ( (
 ( 1.000000000000000000, 0.8047781103519401347, 1.000000000000000000),
 ( 1.000000000000000000, 0.8123785825609330935, 1.000000000000000000),
 ( 1.000000000000000000, 0.8190671539781644306, 1.000000000000000000),
 ( 1.000000000000000000, 0.8192352254841483994, 1.000000000000000000),
 ( 1.000000000000000000, 0.8126129677206640478, 1.000000000000000000),
 ( 1.000000000000000000, 0.8047712537969730073, 1.000000000000000000) ) ) 
 REPRESENTATION_ITEM ( '' )  SURFACE ( )  );
#11408 = LINE ( 'NONE', #13771, #12903 ) ;
#11409 =( GEOMETRIC_REPRESENTATION_CONTEXT ( 3 ) GLOBAL_UNCERTAINTY_ASSIGNED_CONTEXT ( ( #4846 ) ) GLOBAL_UNIT_ASSIGNED_CONTEXT ( ( #6032, #8234, #10513 ) ) REPRESENTATION_CONTEXT ( 'NONE', 'WORKASPACE' ) );
#11410 = DIRECTION ( 'NONE',  ( -1.000000000000000000, -0.000000000000000000, -0.000000000000000000 ) ) ;
#11411 = ORIENTED_EDGE ( 'NONE', *, *, #11650, .T. ) ;
#11412 = ORIENTED_EDGE ( 'NONE', *, *, #2517, .F. ) ;
#11413 = CARTESIAN_POINT ( 'NONE',  ( 108.6817075744280316, -20.42344490663947809, -32.00000000000002842 ) ) ;
#11414 = DIRECTION ( 'NONE',  ( 0.000000000000000000, 0.000000000000000000, 1.000000000000000000 ) ) ;
#11415 = EDGE_CURVE ( 'NONE', #6358, #6826, #1010, .T. ) ;
#11416 = VECTOR ( 'NONE', #4725, 1000.000000000000000 ) ;
#11417 = PRODUCT_DEFINITION ( 'UNKNOWN', '', #7326, #11134 ) ;
#11418 = EDGE_CURVE ( 'NONE', #14384, #7049, #8905, .T. ) ;
#11419 = ORIENTED_EDGE ( 'NONE', *, *, #11005, .T. ) ;
#11420 = VECTOR ( 'NONE', #12420, 1000.000000000000114 ) ;
#11421 = ORIENTED_EDGE ( 'NONE', *, *, #10726, .T. ) ;
#11422 = PLANE ( 'NONE',  #6251 ) ;
#11423 = DIRECTION ( 'NONE',  ( 0.000000000000000000, -8.482162385747133845E-47, 1.000000000000000000 ) ) ;
#11424 = ORIENTED_EDGE ( 'NONE', *, *, #8331, .T. ) ;
#11425 = CARTESIAN_POINT ( 'NONE',  ( 0.000000000000000000, 0.000000000000000000, -3.699999999999981082 ) ) ;
#11426 = CONICAL_SURFACE ( 'NONE', #5802, 2.445500000000002672, 0.7853981633974423948 ) ;
#11427 = VERTEX_POINT ( 'NONE', #5677 ) ;
#11428 = CIRCLE ( 'NONE', #5131, 2.500000000000002220 ) ;
#11429 = LINE ( 'NONE', #3844, #1267 ) ;
#11430 = DIRECTION ( 'NONE',  ( -0.9701425001453319874, -0.2425356250363328858, 0.000000000000000000 ) ) ;
#11431 = VERTEX_POINT ( 'NONE', #13399 ) ;
#11432 = CARTESIAN_POINT ( 'NONE',  ( 4.132952817037849336, -2.031684012687273722, -3.518979934899746365 ) ) ;
#11433 = FACE_OUTER_BOUND ( 'NONE', #8686, .T. ) ;
#11434 = SHAPE_REPRESENTATION_RELATIONSHIP ( 'NONE' , 'NONE' ,  #7389, #4561 ) ;
#11435 = CARTESIAN_POINT ( 'NONE',  ( 49.55443476855437268, 62.09002498982675888, 25.00000000000000000 ) ) ;
#11436 = CARTESIAN_POINT ( 'NONE',  ( 4.960471971868381402, 4.315143281044153234, 0.6753920894105047701 ) ) ;
#11437 = ORIENTED_EDGE ( 'NONE', *, *, #4883, .T. ) ;
#11438 = DIRECTION ( 'NONE',  ( 1.000000000000000000, 3.286707217423839940E-17, 2.273843122241288053E-18 ) ) ;
#11439 = VECTOR ( 'NONE', #10825, 1000.000000000000000 ) ;
#11440 = ORIENTED_EDGE ( 'NONE', *, *, #14144, .F. ) ;
#11441 = CARTESIAN_POINT ( 'NONE',  ( -108.6817075744280316, -20.42344490663947809, -32.00000000000002842 ) ) ;
#11442 = CARTESIAN_POINT ( 'NONE',  ( 1.560000000000005826, 0.8660254037844428154, -1.500000000000001332 ) ) ;
#11443 = ORIENTED_EDGE ( 'NONE', *, *, #12526, .F. ) ;
#11444 = CARTESIAN_POINT ( 'NONE',  ( 4.873329151231326151, -3.113442849146556668, -2.752175560109257013 ) ) ;
#11445 = VERTEX_POINT ( 'NONE', #7652 ) ;
#11446 = LINE ( 'NONE', #2834, #5169 ) ;
#11447 = ORIENTED_EDGE ( 'NONE', *, *, #10393, .T. ) ;
#11448 = AXIS2_PLACEMENT_3D ( 'NONE', #5736, #4671, #1582 ) ;
#11449 = ORIENTED_EDGE ( 'NONE', *, *, #3743, .F. ) ;
#11450 = AXIS2_PLACEMENT_3D ( 'NONE', #9389, #6080, #8577 ) ;
#11451 = CARTESIAN_POINT ( 'NONE',  ( 4.872568031907684727, -3.130604888704431321, -2.722411753064914564 ) ) ;
#11452 = CARTESIAN_POINT ( 'NONE',  ( 1.560000000000005826, -1.299038105676664223, 0.7500000000000006661 ) ) ;
#11453 = ORIENTED_EDGE ( 'NONE', *, *, #5923, .T. ) ;
#11454 = CARTESIAN_POINT ( 'NONE',  ( -2.104029840979682042E-15, 0.3423821193476805358, -3.499999999999996003 ) ) ;
#11455 = EDGE_CURVE ( 'NONE', #5373, #3729, #9854, .T. ) ;
#11456 = CARTESIAN_POINT ( 'NONE',  ( -997.5739745962155212, 0.000000000000000000, 0.000000000000000000 ) ) ;
#11457 = EDGE_CURVE ( 'NONE', #7155, #3422, #3435, .T. ) ;
#11458 = DIRECTION ( 'NONE',  ( 0.000000000000000000, 0.000000000000000000, 1.000000000000000000 ) ) ;
#11459 = DIRECTION ( 'NONE',  ( 0.000000000000000000, 0.000000000000000000, -1.000000000000000000 ) ) ;
#11460 = CONTEXT_DEPENDENT_SHAPE_REPRESENTATION ( #11773, #6258 ) ;
#11461 = LINE ( 'NONE', #13687, #10292 ) ;
#11462 = CARTESIAN_POINT ( 'NONE',  ( -3.999999999999990674, -2.512220432843131235, -3.169390650195370807 ) ) ;
#11463 = AXIS2_PLACEMENT_3D ( 'NONE', #4879, #4957, #10435 ) ;
#11464 = DIRECTION ( 'NONE',  ( -1.000000000000000000, 0.000000000000000000, 0.000000000000000000 ) ) ;
#11465 = CIRCLE ( 'NONE', #10294, 2.500000000000002220 ) ;
#11466 = CONICAL_SURFACE ( 'NONE', #4248, 6.726859516510133474, 1.221730476396048148 ) ;
#11467 = EDGE_CURVE ( 'NONE', #2841, #12256, #9857, .T. ) ;
#11468 = VERTEX_POINT ( 'NONE', #3373 ) ;
#11469 = LINE ( 'NONE', #8028, #9696 ) ;
#11470 = VERTEX_POINT ( 'NONE', #1155 ) ;
#11471 = ORIENTED_EDGE ( 'NONE', *, *, #14435, .T. ) ;
#11472 = CARTESIAN_POINT ( 'NONE',  ( 71.80728622811317052, -17.99808865627608512, -28.00000000000000000 ) ) ;
#11473 = EDGE_CURVE ( 'NONE', #260, #5068, #2039, .T. ) ;
#11474 = CARTESIAN_POINT ( 'NONE',  ( 0.000000000000000000, 0.000000000000000000, -4.394516984716101859 ) ) ;
#11475 = DIRECTION ( 'NONE',  ( 0.000000000000000000, 0.000000000000000000, -1.000000000000000000 ) ) ;
#11476 = FACE_OUTER_BOUND ( 'NONE', #9374, .T. ) ;
#11477 = DIRECTION ( 'NONE',  ( -1.000000000000000000, 0.000000000000000000, 0.000000000000000000 ) ) ;
#11478 = CARTESIAN_POINT ( 'NONE',  ( 0.000000000000000000, 25.49999999999996803, -45.70000000000000284 ) ) ;
#11479 = CYLINDRICAL_SURFACE ( 'NONE', #1425, 2.500000000000002220 ) ;
#11480 = ORIENTED_EDGE ( 'NONE', *, *, #7715, .F. ) ;
#11481 = VECTOR ( 'NONE', #11108, 1000.000000000000000 ) ;
#11482 = VECTOR ( 'NONE', #5073, 1000.000000000000227 ) ;
#11483 = DIRECTION ( 'NONE',  ( -1.000000000000000000, 0.000000000000000000, 0.000000000000000000 ) ) ;
#11484 = VERTEX_POINT ( 'NONE', #6485 ) ;
#11485 = EDGE_CURVE ( 'NONE', #11488, #3442, #8978, .T. ) ;
#11486 = VERTEX_POINT ( 'NONE', #4330 ) ;
#11487 = ORIENTED_EDGE ( 'NONE', *, *, #5036, .T. ) ;
#11488 = VERTEX_POINT ( 'NONE', #11387 ) ;
#11489 = LINE ( 'NONE', #13779, #9485 ) ;
#11490 = DIRECTION ( 'NONE',  ( 0.000000000000000000, 0.000000000000000000, -1.000000000000000000 ) ) ;
#11491 = COLOUR_RGB ( '', 0.08235294, 0.09019608, 0.10196078) ;
#11492 = AXIS2_PLACEMENT_3D ( 'NONE', #7765, #4571, #13263 ) ;
#11493 = ORIENTED_EDGE ( 'NONE', *, *, #2294, .F. ) ;
#11494 = ORIENTED_EDGE ( 'NONE', *, *, #6645, .F. ) ;
#11495 = CARTESIAN_POINT ( 'NONE',  ( 57.35294117647057277, -1.411764705882362358, 23.00000000000000000 ) ) ;
#11496 = ADVANCED_BREP_SHAPE_REPRESENTATION ( '', ( #6910, #11025 ), #5842 ) ;
#11497 = FACE_OUTER_BOUND ( 'NONE', #5349, .T. ) ;
#11498 = ORIENTED_EDGE ( 'NONE', *, *, #4438, .T. ) ;
#11499 = PRESENTATION_LAYER_ASSIGNMENT (  '', '', ( #3820 ) ) ;
#11500 = EDGE_CURVE ( 'NONE', #2949, #7089, #3753, .T. ) ;
#11501 = FACE_OUTER_BOUND ( 'NONE', #1807, .T. ) ;
#11502 = VERTEX_POINT ( 'NONE', #12556 ) ;
#11503 = AXIS2_PLACEMENT_3D ( 'NONE', #14453, #10050, #3552 ) ;
#11504 = ADVANCED_FACE ( 'NONE', ( #8161 ), #1292, .T. ) ;
#11505 = CIRCLE ( 'NONE', #5884, 2.500000000000002220 ) ;
#11506 = VERTEX_POINT ( 'NONE', #9191 ) ;
#11507 = CARTESIAN_POINT ( 'NONE',  ( 6.938893903907228378E-15, 2.540000000000007585, 1.599999999999990319 ) ) ;
#11508 = CARTESIAN_POINT ( 'NONE',  ( 4.175813232069169878, 2.061359961916364725, 3.570380186727388327 ) ) ;
#11509 = CARTESIAN_POINT ( 'NONE',  ( -5.000000000000001776, -2.886751345948152192, -0.5999999999999894307 ) ) ;
#11510 = DIRECTION ( 'NONE',  ( 0.2425356250363329969, -0.9701425001453318764, -0.000000000000000000 ) ) ;
#11511 = SHAPE_REPRESENTATION_RELATIONSHIP ( 'NONE' , 'NONE' ,  #11805, #14323 ) ;
#11512 = DIRECTION ( 'NONE',  ( 0.000000000000000000, 1.000000000000000000, 0.000000000000000000 ) ) ;
#11513 = DIRECTION ( 'NONE',  ( -0.2425356250363330801, 0.9701425001453319874, 0.000000000000000000 ) ) ;
#11514 = AXIS2_PLACEMENT_3D ( 'NONE', #882, #5353, #13203 ) ;
#11515 = ORIENTED_EDGE ( 'NONE', *, *, #14400, .F. ) ;
#11516 = CARTESIAN_POINT ( 'NONE',  ( -129.3408537872145132, 189.5765550933606107, -9.000000000000007105 ) ) ;
#11517 = LINE ( 'NONE', #6970, #2511 ) ;
#11518 = LINE ( 'NONE', #11442, #8463 ) ;
#11519 = ORIENTED_EDGE ( 'NONE', *, *, #9028, .T. ) ;
#11520 = DIRECTION ( 'NONE',  ( -1.000000000000000000, 0.000000000000000000, 0.000000000000000000 ) ) ;
#11521 = CARTESIAN_POINT ( 'NONE',  ( 4.873329151231340362, 3.113442849146619285, 2.752175560109197505 ) ) ;
#11522 = ADVANCED_FACE ( 'NONE', ( #6918 ), #1361, .F. ) ;
#11523 = ORIENTED_EDGE ( 'NONE', *, *, #4246, .F. ) ;
#11524 = DIRECTION ( 'NONE',  ( 0.000000000000000000, 0.000000000000000000, 1.000000000000000000 ) ) ;
#11525 = ORIENTED_EDGE ( 'NONE', *, *, #9134, .F. ) ;
#11526 = CIRCLE ( 'NONE', #5214, 5.000000000000004441 ) ;
#11527 = VERTEX_POINT ( 'NONE', #12625 ) ;
#11528 = CARTESIAN_POINT ( 'NONE',  ( 118.6817075744280601, 189.5765550933606107, 33.00000000000002842 ) ) ;
#11529 = FACE_OUTER_BOUND ( 'NONE', #4423, .T. ) ;
#11530 = FACE_OUTER_BOUND ( 'NONE', #8700, .T. ) ;
#11531 = CIRCLE ( 'NONE', #4086, 3.000000000000000888 ) ;
#11532 = CARTESIAN_POINT ( 'NONE',  ( 20.00000000000000000, 47.00000000000000000, 25.00000000000000000 ) ) ;
#11533 = SURFACE_STYLE_USAGE ( .BOTH. , #1659 ) ;
#11534 = LINE ( 'NONE', #3868, #9541 ) ;
#11535 =( LENGTH_UNIT ( ) NAMED_UNIT ( * ) SI_UNIT ( .MILLI., .METRE. ) );
#11536 = ORIENTED_EDGE ( 'NONE', *, *, #10446, .T. ) ;
#11537 = DIRECTION ( 'NONE',  ( -0.7071067811865490160, -3.116132877773382125E-17, 0.7071067811865460184 ) ) ;
#11538 = CARTESIAN_POINT ( 'NONE',  ( 5.000000000000000888, -2.426004080355346648, -0.4213009713786307620 ) ) ;
#11539 = DIRECTION ( 'NONE',  ( 1.000000000000000000, 1.665334536937734071E-16, 0.000000000000000000 ) ) ;
#11540 = EDGE_CURVE ( 'NONE', #4996, #6397, #9826, .T. ) ;
#11541 = CIRCLE ( 'NONE', #6160, 3.000000000000000888 ) ;
#11542 = EDGE_CURVE ( 'NONE', #1857, #1693, #11700, .T. ) ;
#11543 = ORIENTED_EDGE ( 'NONE', *, *, #3402, .F. ) ;
#11544 = VERTEX_POINT ( 'NONE', #2401 ) ;
#11545 = DIRECTION ( 'NONE',  ( 0.000000000000000000, 0.000000000000000000, 1.000000000000000000 ) ) ;
#11546 = ORIENTED_EDGE ( 'NONE', *, *, #7803, .T. ) ;
#11547 = ORIENTED_EDGE ( 'NONE', *, *, #1873, .F. ) ;
#11548 = EDGE_CURVE ( 'NONE', #13659, #4373, #2470, .T. ) ;
#11549 = ORIENTED_EDGE ( 'NONE', *, *, #2998, .T. ) ;
#11550 = CARTESIAN_POINT ( 'NONE',  ( 0.000000000000000000, 25.49999999999996803, 0.000000000000000000 ) ) ;
#11551 = CARTESIAN_POINT ( 'NONE',  ( 5.029396762153813150, 2.903723574490930659, -4.451008977024209834 ) ) ;
#11552 = LINE ( 'NONE', #8318, #6519 ) ;
#11553 = CARTESIAN_POINT ( 'NONE',  ( 20.00000000000000000, -5.510910596163090344E-15, -25.00000000000000000 ) ) ;
#11554 = DIRECTION ( 'NONE',  ( -0.000000000000000000, -0.000000000000000000, -1.000000000000000000 ) ) ;
#11555 = LINE ( 'NONE', #4823, #7021 ) ;
#11556 =( NAMED_UNIT ( * ) PLANE_ANGLE_UNIT ( ) SI_UNIT ( $, .RADIAN. ) );
#11557 = CLOSED_SHELL ( 'NONE', ( #1871, #10218, #13952, #2528, #4901, #8604, #10910, #4302, #8990, #14167, #12575, #5418, #6454, #6024 ) ) ;
#11558 = CARTESIAN_POINT ( 'NONE',  ( 30.07694101601105530, 130.0000000000000000, -25.00000000000000000 ) ) ;
#11559 = EDGE_CURVE ( 'NONE', #10405, #6636, #11257, .T. ) ;
#11560 = CARTESIAN_POINT ( 'NONE',  ( 2.000000000000001776, -3.464101615137764156, 0.000000000000000000 ) ) ;
#11561 = DIRECTION ( 'NONE',  ( 0.000000000000000000, 0.000000000000000000, -1.000000000000000000 ) ) ;
#11562 = EDGE_CURVE ( 'NONE', #8969, #3225, #5888, .T. ) ;
#11563 = ORIENTED_EDGE ( 'NONE', *, *, #9373, .F. ) ;
#11564 = MANIFOLD_SOLID_BREP ( 'M6 Clearance Hole1', #11557 ) ;
#11565 = CARTESIAN_POINT ( 'NONE',  ( -108.6817075744279748, -20.42344490663957046, 33.00000000000002842 ) ) ;
#11566 = DIRECTION ( 'NONE',  ( -1.000000000000000000, 0.000000000000000000, 0.000000000000000000 ) ) ;
#11567 = EDGE_CURVE ( 'NONE', #12253, #5260, #3584, .T. ) ;
#11568 = EDGE_CURVE ( 'NONE', #10568, #7189, #3799, .T. ) ;
#11569 = ORIENTED_EDGE ( 'NONE', *, *, #4447, .F. ) ;
#11570 = CARTESIAN_POINT ( 'NONE',  ( 20.00000000000000355, 30.00000000000000711, -25.00000000000000000 ) ) ;
#11571 = CARTESIAN_POINT ( 'NONE',  ( 5.103279350327407649, 2.353751664345936412, -4.076817471046929597 ) ) ;
#11572 = ORIENTED_EDGE ( 'NONE', *, *, #7237, .T. ) ;
#11573 = CARTESIAN_POINT ( 'NONE',  ( 88.22284556172391490, -83.66032599071898801, -28.00000000000000000 ) ) ;
#11574 = EDGE_LOOP ( 'NONE', ( #6491, #12437, #5306, #393, #7748, #11421, #13789, #12788 ) ) ;
#11575 = EDGE_LOOP ( 'NONE', ( #3058, #5238, #5947 ) ) ;
#11576 = CARTESIAN_POINT ( 'NONE',  ( -4.211140560182194292, 2.431303136016534250, -3.445885042887453231 ) ) ;
#11577 = LINE ( 'NONE', #6003, #9425 ) ;
#11578 = PLANE ( 'NONE',  #10982 ) ;
#11579 = CARTESIAN_POINT ( 'NONE',  ( 27.75000000000001066, 0.000000000000000000, 0.000000000000000000 ) ) ;
#11580 = CARTESIAN_POINT ( 'NONE',  ( 28.00000000000000355, 29.99999999999999645, 25.00000000000000000 ) ) ;
#11581 = MANIFOLD_SOLID_BREP ( 'TorqueElement', #9457 ) ;
#11582 = EDGE_CURVE ( 'NONE', #4769, #10016, #2117, .T. ) ;
#11583 = DIRECTION ( 'NONE',  ( -0.000000000000000000, -0.000000000000000000, -1.000000000000000000 ) ) ;
#11584 = VERTEX_POINT ( 'NONE', #8304 ) ;
#11585 = SURFACE_SIDE_STYLE ('',( #2749 ) ) ;
#11586 = ORIENTED_EDGE ( 'NONE', *, *, #2139, .F. ) ;
#11587 = DIRECTION ( 'NONE',  ( -1.224646799147353454E-16, 1.000000000000000000, 0.000000000000000000 ) ) ;
#11588 = LINE ( 'NONE', #5943, #9178 ) ;
#11589 = ORIENTED_EDGE ( 'NONE', *, *, #14204, .T. ) ;
#11590 = DIRECTION ( 'NONE',  ( 0.000000000000000000, 1.000000000000000000, 0.000000000000000000 ) ) ;
#11591 = FACE_BOUND ( 'NONE', #14172, .T. ) ;
#11592 = ORIENTED_EDGE ( 'NONE', *, *, #10673, .F. ) ;
#11593 = CARTESIAN_POINT ( 'NONE',  ( 0.000000000000000000, 249.5765550933606391, 4.000000000000003553 ) ) ;
#11594 = ORIENTED_EDGE ( 'NONE', *, *, #13678, .F. ) ;
#11595 = ORIENTED_EDGE ( 'NONE', *, *, #12813, .F. ) ;
#11596 = CIRCLE ( 'NONE', #12312, 1.500000000000000000 ) ;
#11597 = PLANE ( 'NONE',  #1497 ) ;
#11598 = DIRECTION ( 'NONE',  ( 0.000000000000000000, 0.000000000000000000, 1.000000000000000000 ) ) ;
#11599 = ORIENTED_EDGE ( 'NONE', *, *, #917, .F. ) ;
#11600 = CARTESIAN_POINT ( 'NONE',  ( 5.000882498481377780, -2.309401076758483384, 4.000000000000005329 ) ) ;
#11601 = DIRECTION ( 'NONE',  ( -1.000000000000000000, 0.000000000000000000, 0.000000000000000000 ) ) ;
#11602 = CARTESIAN_POINT ( 'NONE',  ( 36.31750732272606541, 144.5765550933605823, 33.00000000000000000 ) ) ;
#11603 = EDGE_CURVE ( 'NONE', #11273, #8228, #9356, .T. ) ;
#11604 = LINE ( 'NONE', #2846, #678 ) ;
#11605 = EDGE_CURVE ( 'NONE', #10601, #5280, #10276, .T. ) ;
#11606 = SURFACE_STYLE_FILL_AREA ( #7134 ) ;
#11607 = ITEM_DEFINED_TRANSFORMATION ( 'NONE', 'NONE', #12470,  #11025 ) ;
#11608 = LINE ( 'NONE', #13899, #500 ) ;
#11609 = DIRECTION ( 'NONE',  ( 0.000000000000000000, 0.000000000000000000, 1.000000000000000000 ) ) ;
#11610 = CARTESIAN_POINT ( 'NONE',  ( 36.99999999999999289, 80.00000000000000000, 23.00000000000000000 ) ) ;
#11611 = DIRECTION ( 'NONE',  ( 0.000000000000000000, -8.482162385747133845E-47, 1.000000000000000000 ) ) ;
#11612 = CIRCLE ( 'NONE', #9286, 2.500000000000002220 ) ;
#11613 = EDGE_CURVE ( 'NONE', #8560, #13436, #6783, .T. ) ;
#11614 = CIRCLE ( 'NONE', #13501, 2.500000000000002220 ) ;
#11615 = ORIENTED_EDGE ( 'NONE', *, *, #14183, .T. ) ;
#11616 = CARTESIAN_POINT ( 'NONE',  ( 4.000000000000003553, 0.000000000000000000, 0.000000000000000000 ) ) ;
#11617 = ORIENTED_EDGE ( 'NONE', *, *, #14366, .T. ) ;
#11618 = ORIENTED_EDGE ( 'NONE', *, *, #9846, .T. ) ;
#11619 = CARTESIAN_POINT ( 'NONE',  ( 25.90000000000000213, 29.99999999999999645, -6.999999999999992006 ) ) ;
#11620 = DIRECTION ( 'NONE',  ( -1.000000000000000000, 0.000000000000000000, 0.000000000000000000 ) ) ;
#11621 = DIRECTION ( 'NONE',  ( 1.000000000000000000, 0.000000000000000000, 0.000000000000000000 ) ) ;
#11622 = CARTESIAN_POINT ( 'NONE',  ( 21.68170757442808849, 141.2731697022877313, -23.00000000000000000 ) ) ;
#11623 = CARTESIAN_POINT ( 'NONE',  ( 5.076540720129291806, -2.330508241952945259, -4.036558682520535513 ) ) ;
#11624 = CONICAL_SURFACE ( 'NONE', #7406, 2.054999999999999716, 0.7853981633974428389 ) ;
#11625 = CARTESIAN_POINT ( 'NONE',  ( 0.02944718078426632191, -0.6813962075685970898, 3.499999999999996003 ) ) ;
#11626 = APPLICATION_PROTOCOL_DEFINITION ( 'draft international standard', 'automotive_design', 1998, #10544 ) ;
#11627 = CARTESIAN_POINT ( 'NONE',  ( -4.197393957002299558, 0.4069871074557444568, -3.203767560748908227 ) ) ;
#11628 = CARTESIAN_POINT ( 'NONE',  ( -129.3408537872145132, 189.5765550933606107, -9.000000000000007105 ) ) ;
#11629 = PRODUCT ( 'connector', 'connector', '', ( #9793 ) ) ;
#11630 = CARTESIAN_POINT ( 'NONE',  ( 0.03421028094652860813, -3.855830693249136853, -1.321505333908961521 ) ) ;
#11631 = CIRCLE ( 'NONE', #7178, 5.000000000000000888 ) ;
#11632 = VECTOR ( 'NONE', #1291, 1000.000000000000000 ) ;
#11633 = VERTEX_POINT ( 'NONE', #6196 ) ;
#11635 = MANIFOLD_SOLID_BREP ( 'Fillet1', #13918 ) ;
#11634 = ADVANCED_FACE ( 'NONE', ( #2930 ), #576, .F. ) ;
#11636 = CARTESIAN_POINT ( 'NONE',  ( 5.005339752383226148, -2.263494164695139421, 4.079513104112300503 ) ) ;
#11637 = CARTESIAN_POINT ( 'NONE',  ( -4.154094228333754302, -2.398367420967508767, -3.421909803043237996 ) ) ;
#11638 = AXIS2_PLACEMENT_3D ( 'NONE', #4928, #2590, #8282 ) ;
#11639 = SHAPE_REPRESENTATION_RELATIONSHIP ( 'NONE' , 'NONE' ,  #3865, #10469 ) ;
#11640 = ADVANCED_FACE ( 'NONE', ( #8602 ), #13090, .T. ) ;
#11641 = ADVANCED_FACE ( 'NONE', ( #4956 ), #6315, .T. ) ;
#11642 = AXIS2_PLACEMENT_3D ( 'NONE', #4107, #13093, #12954 ) ;
#11643 = VECTOR ( 'NONE', #4743, 1000.000000000000000 ) ;
#11644 = ORIENTED_EDGE ( 'NONE', *, *, #13369, .T. ) ;
#11645 = VERTEX_POINT ( 'NONE', #2771 ) ;
#11646 = CARTESIAN_POINT ( 'NONE',  ( 54.40514726928103784, 42.68717498692012668, 25.00000000000000000 ) ) ;
#11647 = CARTESIAN_POINT ( 'NONE',  ( 4.988724804725841011, 2.309401076758504701, -4.000000000000003553 ) ) ;
#11648 = EDGE_LOOP ( 'NONE', ( #791, #4692, #781, #10461 ) ) ;
#11649 = DIRECTION ( 'NONE',  ( 0.000000000000000000, 0.000000000000000000, 1.000000000000000000 ) ) ;
#11650 = EDGE_CURVE ( 'NONE', #6870, #13190, #3294, .T. ) ;
#11651 = VECTOR ( 'NONE', #4384, 999.9999999999998863 ) ;
#11652 = FACE_OUTER_BOUND ( 'NONE', #220, .T. ) ;
#11653 = CARTESIAN_POINT ( 'NONE',  ( 22.00000000000000711, 20.00000000000000355, 25.00000000000000000 ) ) ;
#11654 = FACE_OUTER_BOUND ( 'NONE', #1019, .T. ) ;
#11655 = EDGE_LOOP ( 'NONE', ( #7293, #8313, #6974, #724, #3910, #6601 ) ) ;
#11656 = CARTESIAN_POINT ( 'NONE',  ( 4.175813232069169878, 4.122719923832743660, 0.000000000000000000 ) ) ;
#11657 = FACE_OUTER_BOUND ( 'NONE', #7053, .T. ) ;
#11658 =( LENGTH_UNIT ( ) NAMED_UNIT ( * ) SI_UNIT ( .MILLI., .METRE. ) );
#11659 = VERTEX_POINT ( 'NONE', #3203 ) ;
#11660 = CARTESIAN_POINT ( 'NONE',  ( 3.417629563436334728, 3.800333343455863044, -4.019399823475544586 ) ) ;
#11661 = MANIFOLD_SOLID_BREP ( 'FlangeHexFillet', #8272 ) ;
#11662 = CARTESIAN_POINT ( 'NONE',  ( 36.99999999999999289, 80.00000000000000000, -25.00000000000000000 ) ) ;
#11663 = ORIENTED_EDGE ( 'NONE', *, *, #5466, .F. ) ;
#11664 = DIRECTION ( 'NONE',  ( -0.000000000000000000, -1.000000000000000000, -0.000000000000000000 ) ) ;
#11665 = CARTESIAN_POINT ( 'NONE',  ( 20.00000000000000355, 17.00000000000000000, 25.00000000000000000 ) ) ;
#11666 = AXIS2_PLACEMENT_3D ( 'NONE', #11031, #7945, #1151 ) ;
#11667 = ORIENTED_EDGE ( 'NONE', *, *, #1992, .T. ) ;
#11668 = DIRECTION ( 'NONE',  ( -2.960064101202771857E-17, -0.8660254037844380415, -0.5000000000000012212 ) ) ;
#11669 = CARTESIAN_POINT ( 'NONE',  ( 4.862831555537598049, 2.651660758729716072, 3.407188841443499872 ) ) ;
#11670 = CARTESIAN_POINT ( 'NONE',  ( 22.00000000000000355, 27.00000000000000355, 25.00000000000000000 ) ) ;
#11671 = ORIENTED_EDGE ( 'NONE', *, *, #2079, .F. ) ;
#11672 = EDGE_CURVE ( 'NONE', #7122, #13364, #8886, .T. ) ;
#11673 = ORIENTED_EDGE ( 'NONE', *, *, #1235, .T. ) ;
#11674 = LINE ( 'NONE', #13890, #2426 ) ;
#11675 = DIRECTION ( 'NONE',  ( 0.000000000000000000, 1.000000000000000000, 0.000000000000000000 ) ) ;
#11676 = ORIENTED_EDGE ( 'NONE', *, *, #12017, .F. ) ;
#11677 = CARTESIAN_POINT ( 'NONE',  ( 4.158413352280787123, -4.089743253945648860, -1.387778780781445676E-14 ) ) ;
#11678 = VECTOR ( 'NONE', #14195, 1000.000000000000000 ) ;
#11679 = CARTESIAN_POINT ( 'NONE',  ( -7.836748827996783582E-15, -3.268109542640645682, 2.339468227445697046 ) ) ;
#11680 =( NAMED_UNIT ( * ) PLANE_ANGLE_UNIT ( ) SI_UNIT ( $, .RADIAN. ) );
#11681 = DIRECTION ( 'NONE',  ( -0.000000000000000000, -0.000000000000000000, -1.000000000000000000 ) ) ;
#11682 = CYLINDRICAL_SURFACE ( 'NONE', #4257, 2.500000000000002220 ) ;
#11683 = CARTESIAN_POINT ( 'NONE',  ( 28.00000000000000355, 29.99999999999999645, 25.00000000000000000 ) ) ;
#11684 = DIRECTION ( 'NONE',  ( 0.000000000000000000, 0.000000000000000000, 1.000000000000000000 ) ) ;
#11685 = CARTESIAN_POINT ( 'NONE',  ( 24.99999999999998934, -30.42444490663959300, -2.000000000000001776 ) ) ;
#11686 = MANIFOLD_SOLID_BREP ( 'Mirror2', #10858 ) ;
#11687 = AXIS2_PLACEMENT_3D ( 'NONE', #1808, #5308, #4233 ) ;
#11688 = EDGE_CURVE ( 'NONE', #1738, #981, #4259, .T. ) ;
#11689 = EDGE_CURVE ( 'NONE', #12513, #13862, #2176, .T. ) ;
#11690 = EDGE_LOOP ( 'NONE', ( #1251, #6468, #5874, #6457 ) ) ;
#11691 = CARTESIAN_POINT ( 'NONE',  ( 1.560000000000005826, 0.8660254037844428154, 1.500000000000001332 ) ) ;
#11692 = ORIENTED_EDGE ( 'NONE', *, *, #1189, .T. ) ;
#11693 = ORIENTED_EDGE ( 'NONE', *, *, #3890, .T. ) ;
#11694 = PLANE ( 'NONE',  #11214 ) ;
#11695 = DIRECTION ( 'NONE',  ( -1.000000000000000000, -1.224646799147353454E-16, 0.000000000000000000 ) ) ;
#11696 = DIRECTION ( 'NONE',  ( -1.000000000000000000, -0.000000000000000000, -0.000000000000000000 ) ) ;
#11697 = CYLINDRICAL_SURFACE ( 'NONE', #1967, 2.500000000000002220 ) ;
#11698 = CONICAL_SURFACE ( 'NONE', #13579, 2.450000000000000622, 0.9599310885968804774 ) ;
#11699 = CARTESIAN_POINT ( 'NONE',  ( 39.77836601746437850, 91.19429999418670718, -25.00000000000000000 ) ) ;
#11700 = CIRCLE ( 'NONE', #13121, 8.000000000000000000 ) ;
#11701 = VERTEX_POINT ( 'NONE', #11012 ) ;
#11702 = VECTOR ( 'NONE', #5289, 1000.000000000000000 ) ;
#11703 = CARTESIAN_POINT ( 'NONE',  ( 5.733169058567799681, -9.797989565831383431E-15, -6.438111078829122036 ) ) ;
#11704 = DIRECTION ( 'NONE',  ( -5.551115123125782702E-17, -2.775557561562891351E-17, 1.000000000000000000 ) ) ;
#11705 = DIRECTION ( 'NONE',  ( -1.000000000000000000, 0.000000000000000000, 0.000000000000000000 ) ) ;
#11706 = VECTOR ( 'NONE', #7105, 1000.000000000000000 ) ;
#11707 = CARTESIAN_POINT ( 'NONE',  ( 4.175813232069169878, 2.061359961916364725, 3.570380186727388327 ) ) ;
#11708 = AXIS2_PLACEMENT_3D ( 'NONE', #3063, #7490, #13911 ) ;
#11709 = LINE ( 'NONE', #5270, #11992 ) ;
#11710 = VECTOR ( 'NONE', #8103, 1000.000000000000000 ) ;
#11711 = ORIENTED_EDGE ( 'NONE', *, *, #3876, .T. ) ;
#11712 = VECTOR ( 'NONE', #1279, 1000.000000000000000 ) ;
#11713 = EDGE_CURVE ( 'NONE', #6044, #6152, #248, .T. ) ;
#11714 = EDGE_LOOP ( 'NONE', ( #2664, #7767, #6625, #6750 ) ) ;
#11715 = MANIFOLD_SOLID_BREP ( '<Hardened Serrated Safety Wedge>-<AdvancedHole1>', #6176 ) ;
#11717 = ORIENTED_EDGE ( 'NONE', *, *, #3601, .T. ) ;
#11716 = AXIS2_PLACEMENT_3D ( 'NONE', #12456, #7455, #9371 ) ;
#11718 = CARTESIAN_POINT ( 'NONE',  ( 1.560000000000005826, -1.732050807568885631, 0.000000000000000000 ) ) ;
#11719 = DIRECTION ( 'NONE',  ( 0.000000000000000000, 0.000000000000000000, 1.000000000000000000 ) ) ;
#11720 = AXIS2_PLACEMENT_3D ( 'NONE', #3961, #861, #7380 ) ;
#11721 = ORIENTED_EDGE ( 'NONE', *, *, #11046, .T. ) ;
#11722 = MECHANICAL_DESIGN_GEOMETRIC_PRESENTATION_REPRESENTATION (  '', ( #3555 ), #13142 ) ;
#11723 = AXIS2_PLACEMENT_3D ( 'NONE', #6355, #1980, #14205 ) ;
#11724 = ORIENTED_EDGE ( 'NONE', *, *, #10428, .F. ) ;
#11725 = LINE ( 'NONE', #5058, #12566 ) ;
#11726 = CARTESIAN_POINT ( 'NONE',  ( 0.1702248550645342196, -5.871782057790571940, -4.589066185948686538 ) ) ;
#11727 = ORIENTED_EDGE ( 'NONE', *, *, #6776, .F. ) ;
#11728 = B_SPLINE_CURVE_WITH_KNOTS ( 'NONE', 3,
 ( #982, #8594, #5447, #10729, #12184, #9919, #9628, #11905 ),
 .UNSPECIFIED., .F., .F.,
 ( 4, 2, 2, 4 ),
 ( 0.000000000000000000, 0.002450665683189818828, 0.003675998524784728459, 0.004901331366379637657 ),
 .UNSPECIFIED. ) ;
#11729 = LINE ( 'NONE', #4918, #774 ) ;
#11730 = EDGE_CURVE ( 'NONE', #9429, #1767, #12054, .T. ) ;
#11731 = VECTOR ( 'NONE', #11675, 1000.000000000000000 ) ;
#11732 = ORIENTED_EDGE ( 'NONE', *, *, #14255, .F. ) ;
#11733 = AXIS2_PLACEMENT_3D ( 'NONE', #13864, #12522, #12590 ) ;
#11734 = VECTOR ( 'NONE', #5291, 1000.000000000000114 ) ;
#11735 = CARTESIAN_POINT ( 'NONE',  ( 1.560000000000005826, 0.8660254037844428154, -1.500000000000001332 ) ) ;
#11736 = DIRECTION ( 'NONE',  ( -0.2425356250363330801, 0.9701425001453319874, 0.000000000000000000 ) ) ;
#11737 = DIRECTION ( 'NONE',  ( 0.000000000000000000, -1.000000000000000000, 0.000000000000000000 ) ) ;
#11738 = ORIENTED_EDGE ( 'NONE', *, *, #3162, .F. ) ;
#11739 = CARTESIAN_POINT ( 'NONE',  ( 4.104070371397483541, 4.047367226856751543, -1.387778780781445676E-14 ) ) ;
#11740 = CARTESIAN_POINT ( 'NONE',  ( 40.00000000000000711, 80.00000000000000000, -25.00000000000000000 ) ) ;
#11741 = ORIENTED_EDGE ( 'NONE', *, *, #1838, .F. ) ;
#11742 = CARTESIAN_POINT ( 'NONE',  ( 0.000000000000000000, 249.5765550933606391, 4.000000000000003553 ) ) ;
#11743 = LINE ( 'NONE', #5938, #10330 ) ;
#11744 = CARTESIAN_POINT ( 'NONE',  ( 4.630153689607063860, -2.981509523526843174E-16, -5.371010071662830399 ) ) ;
#11745 = LINE ( 'NONE', #10571, #9570 ) ;
#11746 = ADVANCED_FACE ( 'NONE', ( #4858 ), #2127, .T. ) ;
#11747 = CIRCLE ( 'NONE', #14103, 3.000000000000000888 ) ;
#11748 = CIRCLE ( 'NONE', #2175, 4.750000000000000000 ) ;
#11749 = DIRECTION ( 'NONE',  ( 1.000000000000000000, 0.000000000000000000, 0.000000000000000000 ) ) ;
#11750 = VERTEX_POINT ( 'NONE', #13726 ) ;
#11751 = CARTESIAN_POINT ( 'NONE',  ( 21.68170757442808849, 141.2731697022877313, -23.00000000000000000 ) ) ;
#11752 = B_SPLINE_CURVE_WITH_KNOTS ( 'NONE', 3,
 ( #4213, #893, #8654, #13144, #6238 ),
 .UNSPECIFIED., .F., .F.,
 ( 4, 1, 4 ),
 ( 0.000000000000000000, 0.002309401076758504923, 0.004618802153517009845 ),
 .UNSPECIFIED. ) ;
#11753 = CARTESIAN_POINT ( 'NONE',  ( -3.999999999999996447, 1.539600717838993882, -3.000726591567075108 ) ) ;
#11754 = EDGE_CURVE ( 'NONE', #8562, #5249, #6760, .T. ) ;
#11755 = DIRECTION ( 'NONE',  ( 0.000000000000000000, -0.000000000000000000, 1.000000000000000000 ) ) ;
#11756 = ORIENTED_EDGE ( 'NONE', *, *, #10353, .F. ) ;
#11757 = VERTEX_POINT ( 'NONE', #3566 ) ;
#11758 = FACE_OUTER_BOUND ( 'NONE', #10554, .T. ) ;
#11759 = DIRECTION ( 'NONE',  ( 0.000000000000000000, -5.551115123125782702E-17, -1.000000000000000000 ) ) ;
#11760 = ORIENTED_EDGE ( 'NONE', *, *, #13902, .T. ) ;
#11761 = CARTESIAN_POINT ( 'NONE',  ( 22.00000000000000355, 50.00000000000000000, -25.00000000000000000 ) ) ;
#11762 = AXIS2_PLACEMENT_3D ( 'NONE', #8630, #10618, #3160 ) ;
#11763 = PRODUCT_DEFINITION_SHAPE ( 'NONE', 'NONE',  #14472 ) ;
#11764 = CARTESIAN_POINT ( 'NONE',  ( 49.47979101891770171, 52.38859998837343568, -25.00000000000000000 ) ) ;
#11765 = FACE_OUTER_BOUND ( 'NONE', #5136, .T. ) ;
#11766 = CARTESIAN_POINT ( 'NONE',  ( -108.6817075744279748, -20.42344490663957046, 33.00000000000002842 ) ) ;
#11767 = ORIENTED_EDGE ( 'NONE', *, *, #7283, .T. ) ;
#11768 = DIRECTION ( 'NONE',  ( -1.000000000000000000, 0.000000000000000000, 0.000000000000000000 ) ) ;
#11769 = DIRECTION ( 'NONE',  ( 0.000000000000000000, 0.000000000000000000, -1.000000000000000000 ) ) ;
#11770 = CARTESIAN_POINT ( 'NONE',  ( 4.630153689607063860, 0.000000000000000000, 0.000000000000000000 ) ) ;
#11771 = ADVANCED_FACE ( 'NONE', ( #5862 ), #12413, .F. ) ;
#11772 = DIRECTION ( 'NONE',  ( -1.000000000000000000, 0.000000000000000000, 0.000000000000000000 ) ) ;
#11773 =( REPRESENTATION_RELATIONSHIP ('NONE','NONE', #10295, #8883 ) REPRESENTATION_RELATIONSHIP_WITH_TRANSFORMATION ( #11607 )SHAPE_REPRESENTATION_RELATIONSHIP( ) );
#11774 = VECTOR ( 'NONE', #5850, 1000.000000000000000 ) ;
#11775 = ORIENTED_EDGE ( 'NONE', *, *, #11801, .T. ) ;
#11776 = TOROIDAL_SURFACE ( 'NONE', #1018, 5.200000000000001066, 0.4999999999999975020 ) ;
#11777 = DIRECTION ( 'NONE',  ( 1.000000000000000000, -0.000000000000000000, 0.000000000000000000 ) ) ;
#11778 = ORIENTED_EDGE ( 'NONE', *, *, #7208, .F. ) ;
#11779 = EDGE_LOOP ( 'NONE', ( #12405, #8118, #9304, #12204 ) ) ;
#11780 = DIRECTION ( 'NONE',  ( 0.000000000000000000, 1.000000000000000000, 0.000000000000000000 ) ) ;
#11781 = LINE ( 'NONE', #12724, #2327 ) ;
#11782 = AXIS2_PLACEMENT_3D ( 'NONE', #3313, #9959, #4419 ) ;
#11783 = CARTESIAN_POINT ( 'NONE',  ( 2.018703368236236972, 48.24437551459758566, 7.463024472244906171 ) ) ;
#11784 = PLANE ( 'NONE',  #13597 ) ;
#11785 = FACE_OUTER_BOUND ( 'NONE', #10216, .T. ) ;
#11786 = SHAPE_DEFINITION_REPRESENTATION ( #12805, #8883 ) ;
#11787 = PLANE ( 'NONE',  #13849 ) ;
#11788 = EDGE_CURVE ( 'NONE', #10382, #7417, #13589, .T. ) ;
#11789 = CARTESIAN_POINT ( 'NONE',  ( 129.3408537872138595, 189.5765550933606107, -75.00000000000001421 ) ) ;
#11790 = VECTOR ( 'NONE', #7127, 1000.000000000000000 ) ;
#11791 = ORIENTED_EDGE ( 'NONE', *, *, #14426, .F. ) ;
#11792 = DIRECTION ( 'NONE',  ( 0.000000000000000000, 0.000000000000000000, 1.000000000000000000 ) ) ;
#11793 = VERTEX_POINT ( 'NONE', #10349 ) ;
#11794 = ORIENTED_EDGE ( 'NONE', *, *, #9758, .F. ) ;
#11795 = ORIENTED_EDGE ( 'NONE', *, *, #13033, .T. ) ;
#11796 = CARTESIAN_POINT ( 'NONE',  ( 36.31750732272606541, 144.5765550933605823, -33.00000000000000000 ) ) ;
#11797 = CARTESIAN_POINT ( 'NONE',  ( 4.050880675075968718, 1.379097446046174458, 3.567934390854421434 ) ) ;
#11798 = CLOSED_SHELL ( 'NONE', ( #13594, #1629, #2876, #12309, #3171, #5347, #10157, #5803, #11863, #12955, #6544, #6727, #1020, #6414, #912, #2956, #9730, #7866, #13894, #10012, #9732, #2721, #8345, #3879, #10662 ) ) ;
#11799 = ADVANCED_FACE ( 'NONE', ( #330 ), #9245, .F. ) ;
#11800 = ORIENTED_EDGE ( 'NONE', *, *, #2411, .T. ) ;
#11801 = EDGE_CURVE ( 'NONE', #9561, #1257, #6902, .T. ) ;
#11802 = CARTESIAN_POINT ( 'NONE',  ( 3.401922400370089417, -3.809401878280050724, -4.271474537231044089 ) ) ;
#11803 = CARTESIAN_POINT ( 'NONE',  ( 0.03111943836866019192, -6.084399642271201891, -4.666192694417985010 ) ) ;
#11804 = ORIENTED_EDGE ( 'NONE', *, *, #10855, .F. ) ;
#11805 = SHAPE_REPRESENTATION ( 'Cast Steel Wedge Housing Block', ( #11025 ), #532 ) ;
#11806 = CARTESIAN_POINT ( 'NONE',  ( 0.000000000000000000, 0.000000000000000000, 0.000000000000000000 ) ) ;
#11807 = EDGE_CURVE ( 'NONE', #3362, #1210, #2382, .T. ) ;
#11808 = ORIENTED_EDGE ( 'NONE', *, *, #11473, .F. ) ;
#11809 = CARTESIAN_POINT ( 'NONE',  ( 1.560000000000005826, 1.299038105676664223, -0.7500000000000006661 ) ) ;
#11810 = CARTESIAN_POINT ( 'NONE',  ( 31.38313257588132288, 143.6985259526512948, 33.00000000000000000 ) ) ;
#11811 = LINE ( 'NONE', #12752, #13489 ) ;
#11812 = ORIENTED_EDGE ( 'NONE', *, *, #11024, .T. ) ;
#11813 = CARTESIAN_POINT ( 'NONE',  ( 2.500000000000003553, 4.330127018922198978, -3.920524600599840426 ) ) ;
#11814 = CARTESIAN_POINT ( 'NONE',  ( 0.000000000000000000, 1.732050807568871864, 0.000000000000000000 ) ) ;
#11815 = FILL_AREA_STYLE_COLOUR ( '', #5203 ) ;
#11816 = ORIENTED_EDGE ( 'NONE', *, *, #799, .F. ) ;
#11817 = CARTESIAN_POINT ( 'NONE',  ( 5.108705940669683088, 2.340113889544011894, -4.101834868599443240 ) ) ;
#11818 = CIRCLE ( 'NONE', #9300, 4.750000000000000000 ) ;
#11819 = FACE_OUTER_BOUND ( 'NONE', #2967, .T. ) ;
#11820 = ORIENTED_EDGE ( 'NONE', *, *, #9846, .F. ) ;
#11821 = EDGE_CURVE ( 'NONE', #4176, #11002, #11465, .T. ) ;
#11822 = EDGE_CURVE ( 'NONE', #2838, #11484, #5788, .T. ) ;
#11823 = ORIENTED_EDGE ( 'NONE', *, *, #13420, .T. ) ;
#11824 = DIRECTION ( 'NONE',  ( 0.000000000000000000, 0.000000000000000000, -1.000000000000000000 ) ) ;
#11825 = CARTESIAN_POINT ( 'NONE',  ( 105.6817075744280743, 59.57655509336061073, 25.00000000000000000 ) ) ;
#11826 = ORIENTED_EDGE ( 'NONE', *, *, #10228, .T. ) ;
#11827 = DIRECTION ( 'NONE',  ( 1.665334536937734071E-16, -1.000000000000000000, 0.000000000000000000 ) ) ;
#11828 = FACE_BOUND ( 'NONE', #9377, .T. ) ;
#11829 = EDGE_CURVE ( 'NONE', #10062, #4904, #6967, .T. ) ;
#11830 = CARTESIAN_POINT ( 'NONE',  ( 22.00000000000000355, 37.00000000000000711, -25.00000000000000000 ) ) ;
#11831 = DIRECTION ( 'NONE',  ( 0.000000000000000000, 0.000000000000000000, 1.000000000000000000 ) ) ;
#11832 = CARTESIAN_POINT ( 'NONE',  ( -1.738710530748201144, -5.045296470309997616, -4.385927688751861453 ) ) ;
#11833 = ADVANCED_FACE ( 'NONE', ( #9170 ), #8139, .T. ) ;
#11834 = ORIENTED_EDGE ( 'NONE', *, *, #12024, .F. ) ;
#11835 = CARTESIAN_POINT ( 'NONE',  ( 4.165266963751705909, -4.099263933823995565, -1.412887983188416289E-14 ) ) ;
#11836 = CARTESIAN_POINT ( 'NONE',  ( -0.8333333333333353687, -5.292377467571613536, -4.118275046351175028 ) ) ;
#11837 = PLANE ( 'NONE',  #188 ) ;
#11838 = ORIENTED_EDGE ( 'NONE', *, *, #13545, .F. ) ;
#11839 = SURFACE_SIDE_STYLE ('',( #9495 ) ) ;
#11840 = EDGE_CURVE ( 'NONE', #10361, #3683, #9838, .T. ) ;
#11841 = ADVANCED_FACE ( 'NONE', ( #10417 ), #3544, .F. ) ;
#11842 = CARTESIAN_POINT ( 'NONE',  ( 71.80728622811317052, -17.99808865627607801, -25.00000000000000000 ) ) ;
#11843 = CARTESIAN_POINT ( 'NONE',  ( 1.312671235360379107, 3.860931062424219462, -0.05923475698270710271 ) ) ;
#11844 = EDGE_LOOP ( 'NONE', ( #10269, #2577, #2009, #13284 ) ) ;
#11845 = CARTESIAN_POINT ( 'NONE',  ( 59.10586122665984732, -20.42344490663941414, -35.00000000000000000 ) ) ;
#11846 = ORIENTED_EDGE ( 'NONE', *, *, #6614, .F. ) ;
#11847 = EDGE_CURVE ( 'NONE', #7126, #780, #12685, .T. ) ;
#11848 = EDGE_CURVE ( 'NONE', #5579, #8757, #5660, .T. ) ;
#11849 = EDGE_LOOP ( 'NONE', ( #1120, #234, #3445, #6642 ) ) ;
#11850 = DIRECTION ( 'NONE',  ( -1.000000000000000000, 0.000000000000000000, 0.000000000000000000 ) ) ;
#11851 = CARTESIAN_POINT ( 'NONE',  ( 20.00000000000000000, -5.510910596163090344E-15, 25.00000000000000000 ) ) ;
#11852 = CARTESIAN_POINT ( 'NONE',  ( 3.464648251117637301, 47.71258338693829160, 1.984273587230469982 ) ) ;
#11853 = LINE ( 'NONE', #10531, #2600 ) ;
#11854 = CIRCLE ( 'NONE', #5528, 300.0000000000001137 ) ;
#11855 = DIRECTION ( 'NONE',  ( 0.000000000000000000, 0.000000000000000000, -1.000000000000000000 ) ) ;
#11856 = PRODUCT_CONTEXT ( 'NONE', #14381, 'mechanical' ) ;
#11857 = DIRECTION ( 'NONE',  ( 0.000000000000000000, 0.000000000000000000, -1.000000000000000000 ) ) ;
#11858 = DIRECTION ( 'NONE',  ( -1.000000000000000000, 2.551526159633733968E-19, 1.987661601597216239E-18 ) ) ;
#11859 = VECTOR ( 'NONE', #5919, 1000.000000000000000 ) ;
#11860 = CARTESIAN_POINT ( 'NONE',  ( 22.00000000000000000, 78.00000000000000000, -25.00000000000000000 ) ) ;
#11861 = ORIENTED_EDGE ( 'NONE', *, *, #6864, .F. ) ;
#11862 = ORIENTED_EDGE ( 'NONE', *, *, #13345, .T. ) ;
#11863 = ADVANCED_FACE ( 'NONE', ( #13513 ), #9550, .T. ) ;
#11864 = ORIENTED_EDGE ( 'NONE', *, *, #12501, .T. ) ;
#11865 = AXIS2_PLACEMENT_3D ( 'NONE', #10273, #5870, #10356 ) ;
#11866 = FACE_OUTER_BOUND ( 'NONE', #7487, .T. ) ;
#11867 = CARTESIAN_POINT ( 'NONE',  ( 34.85300976710104948, 100.8957249956400375, 25.00000000000000000 ) ) ;
#11868 = ORIENTED_EDGE ( 'NONE', *, *, #13259, .T. ) ;
#11869 = CIRCLE ( 'NONE', #1334, 6.532899837730830939 ) ;
#11870 = CARTESIAN_POINT ( 'NONE',  ( 4.296971609537261649, -3.292644976429659476, -4.396693167837900873 ) ) ;
#11871 = CONICAL_SURFACE ( 'NONE', #13053, 6.726859516510133474, 1.221730476396048148 ) ;
#11872 = CARTESIAN_POINT ( 'NONE',  ( -0.6806757771993166006, -5.380514348699412253, -4.138711833383711181 ) ) ;
#11873 = ORIENTED_EDGE ( 'NONE', *, *, #7659, .T. ) ;
#11874 = DIRECTION ( 'NONE',  ( -1.000000000000000000, 0.000000000000000000, 0.000000000000000000 ) ) ;
#11875 = ORIENTED_EDGE ( 'NONE', *, *, #4070, .T. ) ;
#11876 = ORIENTED_EDGE ( 'NONE', *, *, #8635, .F. ) ;
#11877 = AXIS2_PLACEMENT_3D ( 'NONE', #3693, #10262, #8133 ) ;
#11878 = ORIENTED_EDGE ( 'NONE', *, *, #607, .T. ) ;
#11879 = EDGE_CURVE ( 'NONE', #7309, #8214, #5075, .T. ) ;
#11880 = UNCERTAINTY_MEASURE_WITH_UNIT (LENGTH_MEASURE( 1.000000000000000082E-05 ), #814, 'distance_accuracy_value', 'NONE');
#11881 = PRODUCT_DEFINITION ( 'UNKNOWN', '', #10129, #6438 ) ;
#11882 = EDGE_CURVE ( 'NONE', #7705, #373, #1796, .T. ) ;
#11883 = CARTESIAN_POINT ( 'NONE',  ( 4.000000000000003553, 2.309401076758501592, -3.133295621305376422 ) ) ;
#11884 = CARTESIAN_POINT ( 'NONE',  ( 0.3126073911696169993, -4.041451884327377009, 0.000000000000000000 ) ) ;
#11885 = CARTESIAN_POINT ( 'NONE',  ( 25.39999999999999858, 29.99999999999999645, -34.50000000000000000 ) ) ;
#11886 = VECTOR ( 'NONE', #2700, 1000.000000000000000 ) ;
#11887 = ORIENTED_EDGE ( 'NONE', *, *, #1310, .F. ) ;
#11888 = VECTOR ( 'NONE', #8084, 1000.000000000000000 ) ;
#11889 = CARTESIAN_POINT ( 'NONE',  ( 36.99999999999999289, 80.00000000000000000, -23.00000000000000000 ) ) ;
#11890 = CARTESIAN_POINT ( 'NONE',  ( 4.767562852629141368, -0.8012780123931543264, -4.000000000000002665 ) ) ;
#11891 = ORIENTED_EDGE ( 'NONE', *, *, #13420, .F. ) ;
#11892 = B_SPLINE_CURVE_WITH_KNOTS ( 'NONE', 3,
 ( #2816, #4848, #3907, #2509, #9536, #7253 ),
 .UNSPECIFIED., .F., .F.,
 ( 4, 2, 4 ),
 ( 0.01237452868508166076, 0.01354396209662687284, 0.01471339550817208665 ),
 .UNSPECIFIED. ) ;
#11893 = DIRECTION ( 'NONE',  ( 0.000000000000000000, 0.000000000000000000, -1.000000000000000000 ) ) ;
#11894 = VERTEX_POINT ( 'NONE', #1562 ) ;
#11895 = DIRECTION ( 'NONE',  ( -0.000000000000000000, -0.000000000000000000, -1.000000000000000000 ) ) ;
#11896 = VERTEX_POINT ( 'NONE', #2674 ) ;
#11897 = DIRECTION ( 'NONE',  ( -1.000000000000000000, 0.000000000000000000, 0.000000000000000000 ) ) ;
#11898 = CYLINDRICAL_SURFACE ( 'NONE', #5227, 3.000000000000003553 ) ;
#11899 = ORIENTED_EDGE ( 'NONE', *, *, #7316, .F. ) ;
#11900 = CARTESIAN_POINT ( 'NONE',  ( 1.393927851585489375, -4.043713361053542954, -3.226374918436825112 ) ) ;
#11901 = CARTESIAN_POINT ( 'NONE',  ( 4.851472949721053141, 1.539600717839007205, 4.000000000000032863 ) ) ;
#11902 = VECTOR ( 'NONE', #10286, 1000.000000000000114 ) ;
#11903 = ORIENTED_EDGE ( 'NONE', *, *, #10574, .T. ) ;
#11904 = VERTEX_POINT ( 'NONE', #699 ) ;
#11905 = CARTESIAN_POINT ( 'NONE',  ( -4.211140560182201398, -2.431303136016548017, -3.445885042887453231 ) ) ;
#11906 = CARTESIAN_POINT ( 'NONE',  ( 19.99999999999999645, 67.00000000000000000, 25.00000000000000000 ) ) ;
#11907 = VERTEX_POINT ( 'NONE', #1723 ) ;
#11908 = CARTESIAN_POINT ( 'NONE',  ( 4.158806965674307854, 4.075748668183989842, 0.05940377217583851094 ) ) ;
#11909 = DIRECTION ( 'NONE',  ( 0.000000000000000000, 0.000000000000000000, 1.000000000000000000 ) ) ;
#11910 = CARTESIAN_POINT ( 'NONE',  ( 62.10586122665986863, -20.42344490663937151, 33.00000000000000000 ) ) ;
#11911 = DIRECTION ( 'NONE',  ( 0.000000000000000000, 0.000000000000000000, -1.000000000000000000 ) ) ;
#11912 = VECTOR ( 'NONE', #11696, 1000.000000000000000 ) ;
#11913 = CARTESIAN_POINT ( 'NONE',  ( 4.071447262713911996, -2.020725942163681399, 3.499999999999989342 ) ) ;
#11914 = MANIFOLD_SOLID_BREP ( 'Hex', #12488 ) ;
#11915 = ORIENTED_EDGE ( 'NONE', *, *, #10334, .F. ) ;
#11916 = VERTEX_POINT ( 'NONE', #2906 ) ;
#11917 = ORIENTED_EDGE ( 'NONE', *, *, #4152, .T. ) ;
#11918 = CIRCLE ( 'NONE', #221, 4.600000000000003197 ) ;
#11919 = EDGE_CURVE ( 'NONE', #651, #1507, #6327, .T. ) ;
#11920 = CARTESIAN_POINT ( 'NONE',  ( 2.500000000000018652, 4.330127018922186544, 0.000000000000000000 ) ) ;
#11921 = ORIENTED_EDGE ( 'NONE', *, *, #3513, .F. ) ;
#11922 = ORIENTED_EDGE ( 'NONE', *, *, #14170, .F. ) ;
#11923 = DIRECTION ( 'NONE',  ( -1.000000000000000000, -0.000000000000000000, -0.000000000000000000 ) ) ;
#11924 = VECTOR ( 'NONE', #11475, 1000.000000000000000 ) ;
#11925 = DIRECTION ( 'NONE',  ( -1.000000000000000000, 2.551526159633733968E-19, 1.987661601597216239E-18 ) ) ;
#11926 = CARTESIAN_POINT ( 'NONE',  ( 3.868554393999077412, 47.50270580730570913, 5.050781263000352794 ) ) ;
#11927 = DIRECTION ( 'NONE',  ( 0.000000000000000000, 0.000000000000000000, -1.000000000000000000 ) ) ;
#11928 = CARTESIAN_POINT ( 'NONE',  ( 0.000000000000000000, 40.49999999999999289, 8.000000000000007105 ) ) ;
#11929 = PRODUCT_CONTEXT ( 'NONE', #7067, 'mechanical' ) ;
#11930 = LINE ( 'NONE', #8556, #6585 ) ;
#11931 = CARTESIAN_POINT ( 'NONE',  ( 20.00000000000000000, 47.00000000000000000, 25.00000000000000000 ) ) ;
#11932 = VERTEX_POINT ( 'NONE', #5229 ) ;
#11933 = ADVANCED_FACE ( 'NONE', ( #7344 ), #9475, .F. ) ;
#11934 = CYLINDRICAL_SURFACE ( 'NONE', #2395, 3.000000000000001332 ) ;
#11935 = EDGE_LOOP ( 'NONE', ( #10631, #92, #10180, #6768 ) ) ;
#11936 = EDGE_CURVE ( 'NONE', #7049, #3245, #1640, .T. ) ;
#11937 = VERTEX_POINT ( 'NONE', #7114 ) ;
#11938 = MANIFOLD_SOLID_BREP ( 'Extrude-Thin1', #7814 ) ;
#11939 = ORIENTED_EDGE ( 'NONE', *, *, #1387, .F. ) ;
#11940 = AXIS2_PLACEMENT_3D ( 'NONE', #9017, #9844, #5520 ) ;
#11941 = DIRECTION ( 'NONE',  ( 0.000000000000000000, 0.000000000000000000, -1.000000000000000000 ) ) ;
#11942 = CARTESIAN_POINT ( 'NONE',  ( -4.000000000000000000, -2.309401076758511806, -3.204269196027522693 ) ) ;
#11943 = B_SPLINE_CURVE_WITH_KNOTS ( 'NONE', 3,
 ( #12279, #13394, #5604, #4541, #1435, #3368 ),
 .UNSPECIFIED., .F., .F.,
 ( 4, 2, 4 ),
 ( 0.004308305454211633703, 0.005784651566377418952, 0.007260997678543204201 ),
 .UNSPECIFIED. ) ;
#11944 = ORIENTED_EDGE ( 'NONE', *, *, #7072, .T. ) ;
#11945 = CARTESIAN_POINT ( 'NONE',  ( 0.000000000000000000, 40.49999999999999289, 0.000000000000000000 ) ) ;
#11946 = EDGE_CURVE ( 'NONE', #11896, #7758, #6244, .T. ) ;
#11947 = AXIS2_PLACEMENT_3D ( 'NONE', #9265, #5810, #10289 ) ;
#11948 = PRESENTATION_LAYER_ASSIGNMENT (  '', '', ( #2852 ) ) ;
#11949 = LINE ( 'NONE', #1780, #7508 ) ;
#11950 = DIRECTION ( 'NONE',  ( 0.000000000000000000, 0.000000000000000000, -1.000000000000000000 ) ) ;
#11951 = VECTOR ( 'NONE', #7200, 1000.000000000000000 ) ;
#11952 = ORIENTED_EDGE ( 'NONE', *, *, #6182, .F. ) ;
#11953 = CARTESIAN_POINT ( 'NONE',  ( 42.12907851819100813, 71.79144999128007498, -25.00000000000000000 ) ) ;
#11954 = CARTESIAN_POINT ( 'NONE',  ( 32.50229726637438432, 120.2985749985466839, 25.00000000000000000 ) ) ;
#11955 = CARTESIAN_POINT ( 'NONE',  ( 0.1578711657514496047, -1.548887424847043448, 4.000000000000005329 ) ) ;
#11956 = ORIENTED_EDGE ( 'NONE', *, *, #17, .F. ) ;
#11957 = VECTOR ( 'NONE', #729, 1000.000000000000000 ) ;
#11958 = FACE_OUTER_BOUND ( 'NONE', #8547, .T. ) ;
#11959 = AXIS2_PLACEMENT_3D ( 'NONE', #9796, #8405, #9587 ) ;
#11960 = CARTESIAN_POINT ( 'NONE',  ( 34.92765351673772045, 110.5971499970933536, -25.00000000000000000 ) ) ;
#11961 = SURFACE_STYLE_USAGE ( .BOTH. , #2742 ) ;
#11962 =( REPRESENTATION_RELATIONSHIP ('NONE','NONE', #10295, #1400 ) REPRESENTATION_RELATIONSHIP_WITH_TRANSFORMATION ( #12495 )SHAPE_REPRESENTATION_RELATIONSHIP( ) );
#11963 = PLANE ( 'NONE',  #10799 ) ;
#11964 = VERTEX_POINT ( 'NONE', #11272 ) ;
#11965 = VERTEX_POINT ( 'NONE', #12304 ) ;
#11966 = CARTESIAN_POINT ( 'NONE',  ( 0.3126073911696169993, -4.041451884327377009, 0.000000000000000000 ) ) ;
#11967 = EDGE_CURVE ( 'NONE', #13907, #5068, #13554, .T. ) ;
#11968 = EDGE_CURVE ( 'NONE', #12756, #698, #5319, .T. ) ;
#11969 = LINE ( 'NONE', #8586, #10809 ) ;
#11970 = VERTEX_POINT ( 'NONE', #10172 ) ;
#11971 = CARTESIAN_POINT ( 'NONE',  ( 2.805705207896079578, -3.226868319750171743, -3.203898532754354544 ) ) ;
#11972 = VECTOR ( 'NONE', #4160, 1000.000000000000000 ) ;
#11973 = CARTESIAN_POINT ( 'NONE',  ( -2.540000000000002700, -1.119346853987568578E-16, 1.599999999999990319 ) ) ;
#11974 = VECTOR ( 'NONE', #7100, 1000.000000000000000 ) ;
#11975 = ORIENTED_EDGE ( 'NONE', *, *, #3144, .T. ) ;
#11976 = ORIENTED_EDGE ( 'NONE', *, *, #2768, .F. ) ;
#11977 = DIRECTION ( 'NONE',  ( 0.000000000000000000, 0.000000000000000000, -1.000000000000000000 ) ) ;
#11978 = LINE ( 'NONE', #2920, #11972 ) ;
#11979 = ORIENTED_EDGE ( 'NONE', *, *, #7524, .F. ) ;
#11980 = CARTESIAN_POINT ( 'NONE',  ( -6.532899837730830939, 4.281373044485382480E-15, -6.000000000000005329 ) ) ;
#11981 = DIRECTION ( 'NONE',  ( 0.9701425001453318764, 0.2425356250363329969, 0.000000000000000000 ) ) ;
#11982 = LINE ( 'NONE', #1958, #4638 ) ;
#11983 =( GEOMETRIC_REPRESENTATION_CONTEXT ( 3 ) GLOBAL_UNCERTAINTY_ASSIGNED_CONTEXT ( ( #1784 ) ) GLOBAL_UNIT_ASSIGNED_CONTEXT ( ( #2241, #3487, #42 ) ) REPRESENTATION_CONTEXT ( 'NONE', 'WORKASPACE' ) );
#11984 = LINE ( 'NONE', #1961, #2060 ) ;
#11985 = CIRCLE ( 'NONE', #11492, 4.000000000000000000 ) ;
#11986 = EDGE_LOOP ( 'NONE', ( #4390, #771, #2538, #10634, #3517, #12176 ) ) ;
#11987 = DIRECTION ( 'NONE',  ( 0.000000000000000000, -1.000000000000000000, 0.000000000000000000 ) ) ;
#11988 = PLANE ( 'NONE',  #7890 ) ;
#11989 = EDGE_CURVE ( 'NONE', #10870, #9890, #5694, .T. ) ;
#11990 = DIRECTION ( 'NONE',  ( 0.000000000000000000, 0.000000000000000000, -1.000000000000000000 ) ) ;
#11991 = COLOUR_RGB ( '', 0.72549020, 0.75294118, 0.79215686) ;
#11992 = VECTOR ( 'NONE', #9733, 1000.000000000000000 ) ;
#11993 = VECTOR ( 'NONE', #5055, 1000.000000000000000 ) ;
#11994 = ORIENTED_EDGE ( 'NONE', *, *, #11882, .T. ) ;
#11995 = CARTESIAN_POINT ( 'NONE',  ( 0.3126073911695614882, -2.020725942163792421, -3.500000000000003109 ) ) ;
#11996 = ORIENTED_EDGE ( 'NONE', *, *, #109, .F. ) ;
#11997 = CARTESIAN_POINT ( 'NONE',  ( 0.000000000000000000, -20.42344490663941414, -199.4258611313499330 ) ) ;
#11998 = CARTESIAN_POINT ( 'NONE',  ( 5.253368672218637236, -3.033033817057797510, -4.659491423763650886 ) ) ;
#11999 = DIRECTION ( 'NONE',  ( -1.000000000000000000, -0.000000000000000000, 1.387778780781446169E-16 ) ) ;
#12000 = DIRECTION ( 'NONE',  ( -0.000000000000000000, 0.000000000000000000, 1.000000000000000000 ) ) ;
#12001 = CARTESIAN_POINT ( 'NONE',  ( 76.68170757442801744, 39.57655509336063204, -33.00000000000000000 ) ) ;
#12002 = APPLICATION_PROTOCOL_DEFINITION ( 'draft international standard', 'automotive_design', 1998, #10632 ) ;
#12003 = CARTESIAN_POINT ( 'NONE',  ( 4.211405962802040825, 2.460462805100875450, -3.451298870276212405 ) ) ;
#12004 = VECTOR ( 'NONE', #6076, 1000.000000000000000 ) ;
#12005 = DIRECTION ( 'NONE',  ( 1.000000000000000000, 0.000000000000000000, 0.000000000000000000 ) ) ;
#12006 = AXIS2_PLACEMENT_3D ( 'NONE', #7460, #4136, #5212 ) ;
#12007 = EDGE_CURVE ( 'NONE', #4217, #13079, #11338, .T. ) ;
#12008 = EDGE_CURVE ( 'NONE', #12541, #8749, #13611, .T. ) ;
#12009 = ORIENTED_EDGE ( 'NONE', *, *, #13910, .T. ) ;
#12010 = CARTESIAN_POINT ( 'NONE',  ( 20.00000000000000000, 70.00000000000000000, -25.00000000000000000 ) ) ;
#12011 = AXIS2_PLACEMENT_3D ( 'NONE', #1148, #13675, #12346 ) ;
#12012 = VERTEX_POINT ( 'NONE', #11126 ) ;
#12013 = CARTESIAN_POINT ( 'NONE',  ( 4.960860176462370319, -1.574785417369796159, -4.074727069546307590 ) ) ;
#12014 = PRODUCT_DEFINITION_FORMATION_WITH_SPECIFIED_SOURCE ( 'ANY', '', #1709, .NOT_KNOWN. ) ;
#12015 = LINE ( 'NONE', #3, #8476 ) ;
#12016 = CARTESIAN_POINT ( 'NONE',  ( 0.1388410611046031196, 2.351840044243031613, -2.926493552096015360 ) ) ;
#12017 = EDGE_CURVE ( 'NONE', #8916, #5618, #3526, .T. ) ;
#12018 = DIRECTION ( 'NONE',  ( -1.000000000000000000, -3.286707217423839940E-17, -2.273843122241288053E-18 ) ) ;
#12020 = TOROIDAL_SURFACE ( 'NONE', #5001, 2.699999999999999289, 0.2000000000000000111 ) ;
#12019 =( LENGTH_UNIT ( ) NAMED_UNIT ( * ) SI_UNIT ( .MILLI., .METRE. ) );
#12021 = ORIENTED_EDGE ( 'NONE', *, *, #13772, .F. ) ;
#12022 = EDGE_CURVE ( 'NONE', #5483, #11527, #13143, .T. ) ;
#12023 = LINE ( 'NONE', #5594, #1818 ) ;
#12024 = EDGE_CURVE ( 'NONE', #2625, #641, #3094, .T. ) ;
#12025 = DIRECTION ( 'NONE',  ( -1.000000000000000000, -1.913084959030911013E-15, -0.000000000000000000 ) ) ;
#12026 = CARTESIAN_POINT ( 'NONE',  ( 4.468294295033107599E-15, 5.914763229585228821, -4.581769937709100127 ) ) ;
#12027 = DIRECTION ( 'NONE',  ( -0.000000000000000000, -1.000000000000000000, -0.000000000000000000 ) ) ;
#12028 = ORIENTED_EDGE ( 'NONE', *, *, #6526, .T. ) ;
#12029 = CARTESIAN_POINT ( 'NONE',  ( -5.684607805603229377E-18, 1.673838217086936480E-16, -2.499999999999999112 ) ) ;
#12030 = PLANE ( 'NONE',  #374 ) ;
#12031 = CARTESIAN_POINT ( 'NONE',  ( 95.04167153547044222, -149.6197612287760705, -32.99999999999999289 ) ) ;
#12032 = EDGE_CURVE ( 'NONE', #3683, #6291, #1308, .T. ) ;
#12033 = CARTESIAN_POINT ( 'NONE',  ( 30.60000000000001563, 1.140754157802348188E-16, 2.054999999999999716 ) ) ;
#12034 = CARTESIAN_POINT ( 'NONE',  ( 129.3408537872138595, 189.5765550933606107, -80.00000000000002842 ) ) ;
#12035 = CARTESIAN_POINT ( 'NONE',  ( 42.27836601746437850, 91.19429999418670718, 25.00000000000000000 ) ) ;
#12036 = VERTEX_POINT ( 'NONE', #3238 ) ;
#12037 = PLANE ( 'NONE',  #5762 ) ;
#12038 = ADVANCED_FACE ( 'NONE', ( #10026 ), #13421, .F. ) ;
#12039 = CARTESIAN_POINT ( 'NONE',  ( 2.807096675499392902, -3.225959780909705366, -3.202509183706237827 ) ) ;
#12040 = ORIENTED_EDGE ( 'NONE', *, *, #465, .T. ) ;
#12041 = DIRECTION ( 'NONE',  ( 1.000000000000000000, 0.000000000000000000, 0.000000000000000000 ) ) ;
#12042 = CARTESIAN_POINT ( 'NONE',  ( 4.988724804725896966, 2.309401076758504701, 4.000000000000031086 ) ) ;
#12043 = ORIENTED_EDGE ( 'NONE', *, *, #7811, .T. ) ;
#12044 = EDGE_LOOP ( 'NONE', ( #4049, #8477, #1197, #3632 ) ) ;
#12045 = CARTESIAN_POINT ( 'NONE',  ( 108.6817075744280743, 124.5765550933606107, 25.00000000000000000 ) ) ;
#12046 = CARTESIAN_POINT ( 'NONE',  ( -1.532072935877364915E-15, -6.066067634115591467, -4.659491423763650886 ) ) ;
#12047 = APPLICATION_CONTEXT ( 'automotive_design' ) ;
#12048 = EDGE_CURVE ( 'NONE', #9071, #5687, #6728, .T. ) ;
#12049 = ORIENTED_EDGE ( 'NONE', *, *, #141, .F. ) ;
#12050 = CARTESIAN_POINT ( 'NONE',  ( 3.961551342853731228, -2.319461885623312458, -2.982574167880926996 ) ) ;
#12051 = CARTESIAN_POINT ( 'NONE',  ( 37.27836601746437850, 91.19429999418670718, 25.00000000000000000 ) ) ;
#12052 = CARTESIAN_POINT ( 'NONE',  ( 22.00000000000000355, 50.00000000000000000, 25.00000000000000000 ) ) ;
#12053 = FACE_OUTER_BOUND ( 'NONE', #2886, .T. ) ;
#12054 = LINE ( 'NONE', #9319, #4483 ) ;
#12055 = CYLINDRICAL_SURFACE ( 'NONE', #10919, 4.750000000000000000 ) ;
#12056 = CARTESIAN_POINT ( 'NONE',  ( 20.00000000000000000, 47.00000000000000000, 25.00000000000000000 ) ) ;
#12057 = ORIENTED_EDGE ( 'NONE', *, *, #9668, .T. ) ;
#12058 = B_SPLINE_CURVE_WITH_KNOTS ( 'NONE', 3,
 ( #12193, #6692, #12270, #5458, #8887, #8818, #6543, #1068 ),
 .UNSPECIFIED., .F., .F.,
 ( 4, 2, 2, 4 ),
 ( 2.451332856810596242E-07, 0.001475502392055661437, 0.002213131021440651464, 0.002950759650825642358 ),
 .UNSPECIFIED. ) ;
#12059 = ORIENTED_EDGE ( 'NONE', *, *, #5959, .T. ) ;
#12060 = ORIENTED_EDGE ( 'NONE', *, *, #5890, .F. ) ;
#12061 = CYLINDRICAL_SURFACE ( 'NONE', #10366, 2.750000000000003553 ) ;
#12062 = ADVANCED_FACE ( 'NONE', ( #11193 ), #1035, .F. ) ;
#12063 = EDGE_LOOP ( 'NONE', ( #12677, #8268, #1922 ) ) ;
#12064 = DIRECTION ( 'NONE',  ( 0.000000000000000000, 0.000000000000000000, -1.000000000000000000 ) ) ;
#12065 = ADVANCED_FACE ( 'NONE', ( #10100 ), #14431, .F. ) ;
#12066 = CARTESIAN_POINT ( 'NONE',  ( 5.236872748402769062, -0.5081686017868801697, -4.357689166958461868 ) ) ;
#12067 = CARTESIAN_POINT ( 'NONE',  ( 30.60000000000001563, 0.000000000000000000, 0.000000000000000000 ) ) ;
#12068 = CYLINDRICAL_SURFACE ( 'NONE', #2291, 2.499999999999999112 ) ;
#12069 = DIRECTION ( 'NONE',  ( 0.000000000000000000, 1.000000000000000000, 0.000000000000000000 ) ) ;
#12070 = APPLICATION_PROTOCOL_DEFINITION ( 'draft international standard', 'automotive_design', 1998, #3001 ) ;
#12071 = LINE ( 'NONE', #8836, #13385 ) ;
#12072 = CARTESIAN_POINT ( 'NONE',  ( 4.180231891692623769, -4.134807952925586783, -0.02076457676762514040 ) ) ;
#12073 = EDGE_CURVE ( 'NONE', #4637, #9429, #5492, .T. ) ;
#12074 = ORIENTED_EDGE ( 'NONE', *, *, #2284, .F. ) ;
#12075 = CARTESIAN_POINT ( 'NONE',  ( 79.68170757442804586, 59.57655509336061073, 25.00000000000000000 ) ) ;
#12076 = CARTESIAN_POINT ( 'NONE',  ( 30.60000000000000853, 29.99999999999999645, -34.50000000000000000 ) ) ;
#12077 = EDGE_LOOP ( 'NONE', ( #11180, #6568 ) ) ;
#12078 = VECTOR ( 'NONE', #12314, 1000.000000000000000 ) ;
#12079 = DIRECTION ( 'NONE',  ( 1.000000000000000000, 0.000000000000000000, 0.000000000000000000 ) ) ;
#12080 = CARTESIAN_POINT ( 'NONE',  ( 5.000000000000000888, 0.9888715124523294042, -0.07061148569344773140 ) ) ;
#12081 = CARTESIAN_POINT ( 'NONE',  ( 33.99999999999998579, 80.00000000000000000, 23.00000000000000000 ) ) ;
#12082 = CARTESIAN_POINT ( 'NONE',  ( 5.005210273051236669, 4.664356425837167919, 0.07890231416034156064 ) ) ;
#12083 = ORIENTED_EDGE ( 'NONE', *, *, #7179, .T. ) ;
#12084 = ORIENTED_EDGE ( 'NONE', *, *, #4165, .F. ) ;
#12085 = CARTESIAN_POINT ( 'NONE',  ( 0.000000000000000000, -3.031088913245549854, -1.750000000000001554 ) ) ;
#12086 = DIRECTION ( 'NONE',  ( 0.000000000000000000, 0.000000000000000000, -1.000000000000000000 ) ) ;
#12087 = CIRCLE ( 'NONE', #13967, 2.500000000000002220 ) ;
#12088 = LINE ( 'NONE', #6378, #12242 ) ;
#12089 = ORIENTED_EDGE ( 'NONE', *, *, #7163, .F. ) ;
#12090 = AXIS2_PLACEMENT_3D ( 'NONE', #12948, #8233, #2844 ) ;
#12091 = DIRECTION ( 'NONE',  ( -1.000000000000000000, 0.000000000000000000, 0.000000000000000000 ) ) ;
#12092 = EDGE_CURVE ( 'NONE', #13268, #6118, #3455, .T. ) ;
#12093 = CARTESIAN_POINT ( 'NONE',  ( -5.122335214190880670, 2.957381614792602864, -4.581769937709093909 ) ) ;
#12094 = LINE ( 'NONE', #5502, #6231 ) ;
#12095 = LINE ( 'NONE', #7838, #12078 ) ;
#12096 = EDGE_CURVE ( 'NONE', #10101, #6127, #4422, .T. ) ;
#12097 = CARTESIAN_POINT ( 'NONE',  ( 3.973514160553474284, -3.435084588004187811, 1.181876024140309456 ) ) ;
#12098 = CARTESIAN_POINT ( 'NONE',  ( 4.859320940307197745, -1.605931023280709358, -4.000000000000001776 ) ) ;
#12099 =( NAMED_UNIT ( * ) SI_UNIT ( $, .STERADIAN. ) SOLID_ANGLE_UNIT ( ) );
#12100 = CIRCLE ( 'NONE', #7638, 3.299999999999983391 ) ;
#12101 = FACE_OUTER_BOUND ( 'NONE', #12638, .T. ) ;
#12102 = AXIS2_PLACEMENT_3D ( 'NONE', #1227, #8977, #2260 ) ;
#12103 = ORIENTED_EDGE ( 'NONE', *, *, #1816, .F. ) ;
#12104 = ORIENTED_EDGE ( 'NONE', *, *, #10539, .F. ) ;
#12105 = DIRECTION ( 'NONE',  ( 0.000000000000000000, 0.000000000000000000, -1.000000000000000000 ) ) ;
#12106 = EDGE_LOOP ( 'NONE', ( #4555, #13214, #9233, #5848 ) ) ;
#12107 = DIRECTION ( 'NONE',  ( 1.000000000000000000, 0.000000000000000000, 0.000000000000000000 ) ) ;
#12108 = ADVANCED_FACE ( 'NONE', ( #2563 ), #11479, .T. ) ;
#12109 = FACE_BOUND ( 'NONE', #332, .T. ) ;
#12110 = ORIENTED_EDGE ( 'NONE', *, *, #382, .F. ) ;
#12111 = EDGE_LOOP ( 'NONE', ( #3456, #5313, #2020, #3798 ) ) ;
#12112 = EDGE_CURVE ( 'NONE', #5916, #7437, #11408, .T. ) ;
#12113 = CARTESIAN_POINT ( 'NONE',  ( -24.99999999999998934, 189.5765550933606107, -2.000000000000001776 ) ) ;
#12114 = LINE ( 'NONE', #9988, #12202 ) ;
#12115 = CARTESIAN_POINT ( 'NONE',  ( 4.180345304246196214, 2.049116244671346454, -3.591763845239310804 ) ) ;
#12116 = DIRECTION ( 'NONE',  ( 1.000000000000000000, 1.665334536937734071E-16, 0.000000000000000000 ) ) ;
#12117 = CARTESIAN_POINT ( 'NONE',  ( 118.6817075744280316, 69.57655509336046862, 0.000000000000000000 ) ) ;
#12118 = CARTESIAN_POINT ( 'NONE',  ( 21.68170757442799967, 141.2731697022880155, 28.00000000000000000 ) ) ;
#12119 = EDGE_LOOP ( 'NONE', ( #13176, #11563, #9917, #6936, #2735, #13380, #6909, #3806, #6723, #7027, #10424, #2570, #12043, #6207, #7669, #3324, #8826, #10321, #14327, #4888, #14176, #5723, #13306, #11899, #12292, #5548, #10904, #8709, #3364, #7700 ) ) ;
#12120 = CARTESIAN_POINT ( 'NONE',  ( -5.551115123125782702E-14, 3.464101615137750390, -2.000000000000001776 ) ) ;
#12121 = CARTESIAN_POINT ( 'NONE',  ( 28.00000000000000355, 29.99999999999999645, 8.000000000000007105 ) ) ;
#12122 = EDGE_CURVE ( 'NONE', #10542, #7617, #10538, .T. ) ;
#12123 = ORIENTED_EDGE ( 'NONE', *, *, #9650, .T. ) ;
#12124 = APPLICATION_CONTEXT ( 'automotive_design' ) ;
#12125 = ORIENTED_EDGE ( 'NONE', *, *, #12379, .F. ) ;
#12126 = VERTEX_POINT ( 'NONE', #8186 ) ;
#12127 = DIRECTION ( 'NONE',  ( -2.273843122241289979E-18, 5.551115123125782702E-17, 1.000000000000000000 ) ) ;
#12128 = EDGE_LOOP ( 'NONE', ( #13307, #8520, #10322, #12597 ) ) ;
#12129 = AXIS2_PLACEMENT_3D ( 'NONE', #7932, #12409, #10270 ) ;
#12130 = LINE ( 'NONE', #10143, #6525 ) ;
#12131 = DIRECTION ( 'NONE',  ( 0.000000000000000000, 0.000000000000000000, -1.000000000000000000 ) ) ;
#12132 = LINE ( 'NONE', #1079, #8156 ) ;
#12133 = FACE_OUTER_BOUND ( 'NONE', #7415, .T. ) ;
#12134 = FACE_OUTER_BOUND ( 'NONE', #7621, .T. ) ;
#12135 = CONTEXT_DEPENDENT_SHAPE_REPRESENTATION ( #743, #11763 ) ;
#12136 = CYLINDRICAL_SURFACE ( 'NONE', #10088, 3.299999999999997158 ) ;
#12137 = CARTESIAN_POINT ( 'NONE',  ( 4.988724804725785944, -4.618802153517009401, 0.000000000000000000 ) ) ;
#12138 = EDGE_LOOP ( 'NONE', ( #3994, #2905, #2462, #5152, #7763 ) ) ;
#12139 = ADVANCED_FACE ( 'NONE', ( #12650 ), #1464, .F. ) ;
#12140 = PRODUCT_DEFINITION ( 'UNKNOWN', '', #12694, #9219 ) ;
#12141 = EDGE_CURVE ( 'NONE', #6911, #6532, #67, .T. ) ;
#12142 = DIRECTION ( 'NONE',  ( 1.000000000000000000, 0.000000000000000000, 0.000000000000000000 ) ) ;
#12143 = PRESENTATION_LAYER_ASSIGNMENT (  '', '', ( #3971 ) ) ;
#12144 = ORIENTED_EDGE ( 'NONE', *, *, #12783, .F. ) ;
#12145 = CIRCLE ( 'NONE', #10740, 9.000000000000005329 ) ;
#12146 = ORIENTED_EDGE ( 'NONE', *, *, #161, .T. ) ;
#12147 = ORIENTED_EDGE ( 'NONE', *, *, #1999, .T. ) ;
#12148 = DIRECTION ( 'NONE',  ( 0.000000000000000000, -1.000000000000000000, 0.000000000000000000 ) ) ;
#12149 = CARTESIAN_POINT ( 'NONE',  ( -1.738521435313292063, 5.045405839192970809, -4.385926550512752264 ) ) ;
#12150 = CARTESIAN_POINT ( 'NONE',  ( 30.60000000000001563, 0.000000000000000000, 0.000000000000000000 ) ) ;
#12151 = ORIENTED_EDGE ( 'NONE', *, *, #8517, .T. ) ;
#12152 = DIRECTION ( 'NONE',  ( -0.000000000000000000, 0.000000000000000000, 1.000000000000000000 ) ) ;
#12153 = VECTOR ( 'NONE', #4539, 1000.000000000000000 ) ;
#12154 = CARTESIAN_POINT ( 'NONE',  ( 118.6817075744280316, 69.57655509336046862, 0.000000000000000000 ) ) ;
#12155 =( LENGTH_UNIT ( ) NAMED_UNIT ( * ) SI_UNIT ( .MILLI., .METRE. ) );
#12156 = DIRECTION ( 'NONE',  ( 1.000000000000000000, 1.665334536937734318E-16, 0.000000000000000000 ) ) ;
#12157 = VERTEX_POINT ( 'NONE', #521 ) ;
#12158 = CYLINDRICAL_SURFACE ( 'NONE', #3024, 5.499999999999976907 ) ;
#12159 = DIRECTION ( 'NONE',  ( 0.000000000000000000, 0.000000000000000000, 1.000000000000000000 ) ) ;
#12160 = DIRECTION ( 'NONE',  ( -1.000000000000000000, 0.000000000000000000, 0.000000000000000000 ) ) ;
#12161 = AXIS2_PLACEMENT_3D ( 'NONE', #8236, #8468, #13021 ) ;
#12162 = TOROIDAL_SURFACE ( 'NONE', #7939, 6.532899837730830939, 0.5671001622691684840 ) ;
#12163 = FACE_OUTER_BOUND ( 'NONE', #6012, .T. ) ;
#12164 = CARTESIAN_POINT ( 'NONE',  ( 108.6817075744280316, 39.57655509336063915, 33.00000000000002842 ) ) ;
#12165 = CARTESIAN_POINT ( 'NONE',  ( 22.00000000000000355, 37.00000000000000711, 25.00000000000000000 ) ) ;
#12166 = DIRECTION ( 'NONE',  ( 2.551526159633727709E-19, 1.000000000000000000, -3.216245299353268271E-16 ) ) ;
#12167 = PLANE ( 'NONE',  #4244 ) ;
#12168 = AXIS2_PLACEMENT_3D ( 'NONE', #9114, #10373, #4673 ) ;
#12169 = CYLINDRICAL_SURFACE ( 'NONE', #12196, 4.999999999999976907 ) ;
#12170 = ORIENTED_EDGE ( 'NONE', *, *, #2090, .F. ) ;
#12171 = STYLED_ITEM ( 'NONE', ( #8287 ), #11914 ) ;
#12172 = ORIENTED_EDGE ( 'NONE', *, *, #4198, .T. ) ;
#12173 = CARTESIAN_POINT ( 'NONE',  ( 6.800000000000028244, -6.938893903907228378E-15, 0.000000000000000000 ) ) ;
#12174 = CIRCLE ( 'NONE', #5835, 4.000000000000000000 ) ;
#12175 = EDGE_CURVE ( 'NONE', #1477, #2782, #2719, .T. ) ;
#12176 = ORIENTED_EDGE ( 'NONE', *, *, #12976, .F. ) ;
#12177 = DIRECTION ( 'NONE',  ( -2.081668171172168760E-16, 0.000000000000000000, -1.000000000000000000 ) ) ;
#12178 = VECTOR ( 'NONE', #2022, 1000.000000000000000 ) ;
#12179 = FACE_OUTER_BOUND ( 'NONE', #14038, .T. ) ;
#12180 = ORIENTED_EDGE ( 'NONE', *, *, #3386, .F. ) ;
#12181 = AXIS2_PLACEMENT_3D ( 'NONE', #4118, #6053, #2866 ) ;
#12182 = CIRCLE ( 'NONE', #11723, 4.600000000000003197 ) ;
#12183 = ORIENTED_EDGE ( 'NONE', *, *, #6633, .T. ) ;
#12184 = CARTESIAN_POINT ( 'NONE',  ( -2.804994570502171047, -3.229033611042463114, -3.226374918436821115 ) ) ;
#12185 = CARTESIAN_POINT ( 'NONE',  ( -108.6817075744279748, -20.42344490663957046, -106.9999999999999858 ) ) ;
#12186 = VECTOR ( 'NONE', #8336, 1000.000000000000000 ) ;
#12187 = CYLINDRICAL_SURFACE ( 'NONE', #5611, 2.000000000000001776 ) ;
#12188 = DIRECTION ( 'NONE',  ( -0.000000000000000000, -0.000000000000000000, -1.000000000000000000 ) ) ;
#12189 = DIRECTION ( 'NONE',  ( 0.000000000000000000, -1.000000000000000000, -8.482162385747133845E-47 ) ) ;
#12190 = ADVANCED_FACE ( 'NONE', ( #13847 ), #10315, .T. ) ;
#12191 = CARTESIAN_POINT ( 'NONE',  ( 3.948095570617038419, 0.6965071952232524399, 3.499999999999992895 ) ) ;
#12192 = VERTEX_POINT ( 'NONE', #1605 ) ;
#12193 = CARTESIAN_POINT ( 'NONE',  ( -5.000000000000000000, 2.886751345948124214, -0.5999999999999894307 ) ) ;
#12194 = VECTOR ( 'NONE', #12212, 1000.000000000000000 ) ;
#12195 = AXIS2_PLACEMENT_3D ( 'NONE', #10293, #10375, #12562 ) ;
#12196 = AXIS2_PLACEMENT_3D ( 'NONE', #5506, #9659, #6214 ) ;
#12197 = EDGE_CURVE ( 'NONE', #5014, #13727, #9362, .T. ) ;
#12198 = CARTESIAN_POINT ( 'NONE',  ( 4.055492966679574707, 2.385006769472713728, 3.005124364834414141 ) ) ;
#12199 = ORIENTED_EDGE ( 'NONE', *, *, #230, .F. ) ;
#12200 = ORIENTED_EDGE ( 'NONE', *, *, #4804, .T. ) ;
#12201 = CARTESIAN_POINT ( 'NONE',  ( 22.00000000000000355, 50.00000000000000000, 25.00000000000000000 ) ) ;
#12202 = VECTOR ( 'NONE', #9920, 1000.000000000000000 ) ;
#12203 = PRESENTATION_LAYER_ASSIGNMENT (  '', '', ( #3339 ) ) ;
#12204 = ORIENTED_EDGE ( 'NONE', *, *, #2932, .T. ) ;
#12205 = DIRECTION ( 'NONE',  ( 0.000000000000000000, 0.000000000000000000, 1.000000000000000000 ) ) ;
#12206 = VECTOR ( 'NONE', #7964, 999.9999999999998863 ) ;
#12207 = AXIS2_PLACEMENT_3D ( 'NONE', #2006, #7550, #5436 ) ;
#12208 = CARTESIAN_POINT ( 'NONE',  ( 20.00000000000000000, -5.510910596163090344E-15, 25.00000000000000000 ) ) ;
#12209 = PRESENTATION_STYLE_ASSIGNMENT (( #7730 ) ) ;
#12210 = EDGE_CURVE ( 'NONE', #13323, #5531, #371, .T. ) ;
#12211 = DIRECTION ( 'NONE',  ( 0.8660254037844380415, 0.5000000000000009992, 0.000000000000000000 ) ) ;
#12212 = DIRECTION ( 'NONE',  ( -1.000000000000000000, -0.000000000000000000, -0.000000000000000000 ) ) ;
#12213 = CONTEXT_DEPENDENT_SHAPE_REPRESENTATION ( #9989, #12450 ) ;
#12214 = CARTESIAN_POINT ( 'NONE',  ( 4.203935404774708395, 1.640788256319067662, -3.298453876328925283 ) ) ;
#12215 = LINE ( 'NONE', #3511, #978 ) ;
#12216 = VERTEX_POINT ( 'NONE', #7152 ) ;
#12217 = ORIENTED_EDGE ( 'NONE', *, *, #6137, .T. ) ;
#12218 = EDGE_CURVE ( 'NONE', #6374, #12928, #10456, .T. ) ;
#12219 = VECTOR ( 'NONE', #7602, 1000.000000000000000 ) ;
#12220 = DIRECTION ( 'NONE',  ( -1.000000000000000000, 0.000000000000000000, 0.000000000000000000 ) ) ;
#12222 = EDGE_LOOP ( 'NONE', ( #8689, #2935, #1208, #5764 ) ) ;
#12221 = VECTOR ( 'NONE', #4892, 1000.000000000000000 ) ;
#12223 = VERTEX_POINT ( 'NONE', #9290 ) ;
#12224 = CARTESIAN_POINT ( 'NONE',  ( 20.00000000000000000, 37.00000000000000711, 25.00000000000000000 ) ) ;
#12225 = ORIENTED_EDGE ( 'NONE', *, *, #4645, .T. ) ;
#12226 = FILL_AREA_STYLE_COLOUR ( '', #13301 ) ;
#12227 = CARTESIAN_POINT ( 'NONE',  ( -0.4318028594007581322, 5.811705888748987192, -4.566911319714218820 ) ) ;
#12228 = CARTESIAN_POINT ( 'NONE',  ( 108.6817075744280174, 109.5765550933605113, 1.102182119232617753E-14 ) ) ;
#12229 = EDGE_CURVE ( 'NONE', #3683, #10361, #8682, .T. ) ;
#12230 = DIRECTION ( 'NONE',  ( 0.000000000000000000, -1.000000000000000000, 0.000000000000000000 ) ) ;
#12231 = AXIS2_PLACEMENT_3D ( 'NONE', #2330, #483, #12767 ) ;
#12232 = CARTESIAN_POINT ( 'NONE',  ( 105.6817075744281311, 124.5765550933606107, 25.00000000000000000 ) ) ;
#12233 = FACE_OUTER_BOUND ( 'NONE', #7681, .T. ) ;
#12234 = CARTESIAN_POINT ( 'NONE',  ( 0.000000000000000000, 0.000000000000000000, 0.000000000000000000 ) ) ;
#12235 = CARTESIAN_POINT ( 'NONE',  ( -4.211140560182194292, 2.431303136016534250, -3.445885042887453231 ) ) ;
#12236 = ORIENTED_EDGE ( 'NONE', *, *, #10402, .T. ) ;
#12237 = VERTEX_POINT ( 'NONE', #8327 ) ;
#12238 = CARTESIAN_POINT ( 'NONE',  ( 0.1217565302851009168, -2.351289329882169987, -2.927447417349498426 ) ) ;
#12239 = LINE ( 'NONE', #4428, #6122 ) ;
#12240 = CARTESIAN_POINT ( 'NONE',  ( 0.000000000000000000, 199.5765550933606107, -37.00000000000003553 ) ) ;
#12241 = VERTEX_POINT ( 'NONE', #13700 ) ;
#12242 = VECTOR ( 'NONE', #10777, 1000.000000000000000 ) ;
#12243 = CARTESIAN_POINT ( 'NONE',  ( -1.390214784104929269, -4.043996922316123843, -3.202509183706211182 ) ) ;
#12244 = CARTESIAN_POINT ( 'NONE',  ( 4.844561581013646645, -3.066321291060821963, 2.688975731552646131 ) ) ;
#12245 = DIRECTION ( 'NONE',  ( 0.000000000000000000, -0.000000000000000000, -1.000000000000000000 ) ) ;
#12246 = EDGE_CURVE ( 'NONE', #8446, #11659, #10616, .T. ) ;
#12247 = CARTESIAN_POINT ( 'NONE',  ( 0.000000000000000000, 0.000000000000000000, 0.000000000000000000 ) ) ;
#12248 = EDGE_CURVE ( 'NONE', #6044, #11659, #446, .T. ) ;
#12249 = SHAPE_REPRESENTATION_RELATIONSHIP ( 'NONE' , 'NONE' ,  #4432, #11166 ) ;
#12250 = STYLED_ITEM ( 'NONE', ( #13631 ), #5565 ) ;
#12251 = CARTESIAN_POINT ( 'NONE',  ( 5.098157279264020403, 2.347014727359276520, 4.065148753898767175 ) ) ;
#12252 = VERTEX_POINT ( 'NONE', #9442 ) ;
#12253 = VERTEX_POINT ( 'NONE', #7231 ) ;
#12254 = CARTESIAN_POINT ( 'NONE',  ( 5.551115123125782702E-14, 3.464101615137764156, 2.000000000000001776 ) ) ;
#12255 = AXIS2_PLACEMENT_3D ( 'NONE', #412, #12772, #1510 ) ;
#12256 = VERTEX_POINT ( 'NONE', #11707 ) ;
#12257 = DIRECTION ( 'NONE',  ( -1.000000000000000000, -1.665334536937734071E-16, 0.000000000000000000 ) ) ;
#12258 = VERTEX_POINT ( 'NONE', #3668 ) ;
#12259 = EDGE_LOOP ( 'NONE', ( #4598, #4010, #10710, #11339, #3618 ) ) ;
#12260 = FACE_OUTER_BOUND ( 'NONE', #8601, .T. ) ;
#12261 = DIRECTION ( 'NONE',  ( -1.000000000000000000, 0.000000000000000000, 0.000000000000000000 ) ) ;
#12262 = FACE_OUTER_BOUND ( 'NONE', #5625, .T. ) ;
#12263 = CARTESIAN_POINT ( 'NONE',  ( -2.000000000000001776, -3.464101615137750390, 0.000000000000000000 ) ) ;
#12264 = EDGE_CURVE ( 'NONE', #1477, #2687, #1686, .T. ) ;
#12265 = ADVANCED_FACE ( 'NONE', ( #4761 ), #14272, .T. ) ;
#12266 = CARTESIAN_POINT ( 'NONE',  ( 22.00000000000000000, 60.00000000000000711, 25.00000000000000000 ) ) ;
#12267 = CARTESIAN_POINT ( 'NONE',  ( -8.000000000000000000, 40.49999999999999289, 0.000000000000000000 ) ) ;
#12268 = VERTEX_POINT ( 'NONE', #735 ) ;
#12269 = ORIENTED_EDGE ( 'NONE', *, *, #5255, .F. ) ;
#12270 = CARTESIAN_POINT ( 'NONE',  ( -4.191707736911188142, 3.353419101626346155, -0.2701150775513927460 ) ) ;
#12271 = ADVANCED_FACE ( 'NONE', ( #14068 ), #1833, .T. ) ;
#12272 = CARTESIAN_POINT ( 'NONE',  ( 3.948103430091011834, 3.379418997638845124, 1.146674596025581527 ) ) ;
#12273 = ORIENTED_EDGE ( 'NONE', *, *, #1101, .F. ) ;
#12274 = EDGE_CURVE ( 'NONE', #13954, #8738, #12182, .T. ) ;
#12275 = ORIENTED_EDGE ( 'NONE', *, *, #6735, .F. ) ;
#12276 = EDGE_LOOP ( 'NONE', ( #10565, #7954 ) ) ;
#12277 = LINE ( 'NONE', #61, #12153 ) ;
#12278 = EDGE_CURVE ( 'NONE', #13075, #13851, #13838, .T. ) ;
#12279 = CARTESIAN_POINT ( 'NONE',  ( -5.000000000000001776, -2.886751345948152192, -0.5999999999999894307 ) ) ;
#12280 = ADVANCED_FACE ( 'NONE', ( #10832 ), #806, .F. ) ;
#12281 = DIRECTION ( 'NONE',  ( 0.000000000000000000, 0.000000000000000000, 1.000000000000000000 ) ) ;
#12282 = DIRECTION ( 'NONE',  ( 0.000000000000000000, 1.000000000000000000, 0.000000000000000000 ) ) ;
#12283 = DIRECTION ( 'NONE',  ( -0.9701425001453319874, -0.2425356250363328858, 0.000000000000000000 ) ) ;
#12284 = ITEM_DEFINED_TRANSFORMATION ( 'NONE', 'NONE', #13191,  #11025 ) ;
#12285 = CARTESIAN_POINT ( 'NONE',  ( 30.60000000000001563, 1.375895014445462134E-16, -2.054999999999999716 ) ) ;
#12286 = ADVANCED_FACE ( 'NONE', ( #6489 ), #2863, .T. ) ;
#12287 = CARTESIAN_POINT ( 'NONE',  ( 5.103021810857247154, -4.706811482981973604, 5.672048699061844739E-14 ) ) ;
#12288 = VERTEX_POINT ( 'NONE', #6424 ) ;
#12289 = PLANE ( 'NONE',  #1473 ) ;
#12290 = EDGE_LOOP ( 'NONE', ( #5744, #7404, #6906, #2017, #4167, #4063 ) ) ;
#12291 = EDGE_CURVE ( 'NONE', #7600, #2673, #2602, .T. ) ;
#12292 = ORIENTED_EDGE ( 'NONE', *, *, #9189, .T. ) ;
#12293 = CARTESIAN_POINT ( 'NONE',  ( 0.1404055950190679636, 4.699865361596996749, -3.386887224136954533 ) ) ;
#12294 = ORIENTED_EDGE ( 'NONE', *, *, #13271, .T. ) ;
#12295 = CIRCLE ( 'NONE', #14402, 4.600000000000003197 ) ;
#12296 = VERTEX_POINT ( 'NONE', #12887 ) ;
#12297 = CARTESIAN_POINT ( 'NONE',  ( 22.00000000000000711, 20.00000000000000355, -25.00000000000000000 ) ) ;
#12298 = CARTESIAN_POINT ( 'NONE',  ( 108.6817075744280316, 69.57655509336046862, 3.299999999999976730 ) ) ;
#12299 = FACE_OUTER_BOUND ( 'NONE', #9907, .T. ) ;
#12300 = DIRECTION ( 'NONE',  ( 0.000000000000000000, -8.482162385747133845E-47, 1.000000000000000000 ) ) ;
#12301 = DIRECTION ( 'NONE',  ( 1.000000000000000000, 0.000000000000000000, 0.000000000000000000 ) ) ;
#12302 = FACE_OUTER_BOUND ( 'NONE', #764, .T. ) ;
#12303 =( NAMED_UNIT ( * ) SI_UNIT ( $, .STERADIAN. ) SOLID_ANGLE_UNIT ( ) );
#12304 = CARTESIAN_POINT ( 'NONE',  ( 20.00000000000000000, 27.00000000000000355, -25.00000000000000000 ) ) ;
#12305 = ORIENTED_EDGE ( 'NONE', *, *, #5273, .F. ) ;
#12306 = ORIENTED_EDGE ( 'NONE', *, *, #7835, .F. ) ;
#12307 = DIRECTION ( 'NONE',  ( 1.000000000000000000, 0.000000000000000000, 0.000000000000000000 ) ) ;
#12308 = CARTESIAN_POINT ( 'NONE',  ( 4.000000000000003553, 2.309401076758511806, -0.5000000000000004441 ) ) ;
#12309 = ADVANCED_FACE ( 'NONE', ( #9516 ), #2042, .F. ) ;
#12310 = CARTESIAN_POINT ( 'NONE',  ( 34.92765351673772045, 110.5971499970933536, 25.00000000000000000 ) ) ;
#12311 = ORIENTED_EDGE ( 'NONE', *, *, #7070, .T. ) ;
#12312 = AXIS2_PLACEMENT_3D ( 'NONE', #7466, #6165, #823 ) ;
#12313 = CARTESIAN_POINT ( 'NONE',  ( 5.005210273051227787, -4.664356425837157261, -0.07890231416034962364 ) ) ;
#12314 = DIRECTION ( 'NONE',  ( 0.000000000000000000, 0.000000000000000000, -1.000000000000000000 ) ) ;
#12315 = DIRECTION ( 'NONE',  ( 2.273843122241288438E-18, 5.551115123125783935E-17, 1.000000000000000000 ) ) ;
#12316 = CARTESIAN_POINT ( 'NONE',  ( 3.973514160553477836, -2.741076955031354956, -2.383932505289875881 ) ) ;
#12317 = ORIENTED_EDGE ( 'NONE', *, *, #13904, .F. ) ;
#12318 = B_SPLINE_CURVE_WITH_KNOTS ( 'NONE', 3,
 ( #4632, #5837, #6950, #309, #8114, #3747 ),
 .UNSPECIFIED., .F., .F.,
 ( 4, 2, 4 ),
 ( 0.000000000000000000, 0.0002514304509865763950, 0.0005028609019731527900 ),
 .UNSPECIFIED. ) ;
#12319 = CARTESIAN_POINT ( 'NONE',  ( 0.000000000000000000, 0.000000000000000000, 0.000000000000000000 ) ) ;
#12320 =( LENGTH_UNIT ( ) NAMED_UNIT ( * ) SI_UNIT ( .MILLI., .METRE. ) );
#12321 = CIRCLE ( 'NONE', #12090, 2.500000000000002220 ) ;
#12322 = ORIENTED_EDGE ( 'NONE', *, *, #8507, .T. ) ;
#12323 = EDGE_CURVE ( 'NONE', #1219, #1, #12641, .T. ) ;
#12324 = CARTESIAN_POINT ( 'NONE',  ( 0.3572655899081733644, 2.309401076758511806, 3.999999999999989786 ) ) ;
#12325 = EDGE_CURVE ( 'NONE', #1084, #4217, #7448, .T. ) ;
#12326 = PRODUCT ( 'Cast Steel Wedge Housing Block', 'Cast Steel Wedge Housing Block', '', ( #4261 ) ) ;
#12327 = VERTEX_POINT ( 'NONE', #9728 ) ;
#12328 = ORIENTED_EDGE ( 'NONE', *, *, #5100, .T. ) ;
#12329 = CARTESIAN_POINT ( 'NONE',  ( -5.000000000000000000, 2.886751345948127767, -6.000000000000005329 ) ) ;
#12330 = DIRECTION ( 'NONE',  ( 0.000000000000000000, 0.000000000000000000, 1.000000000000000000 ) ) ;
#12331 = AXIS2_PLACEMENT_3D ( 'NONE', #14452, #13218, #3190 ) ;
#12332 = LINE ( 'NONE', #14459, #9104 ) ;
#12333 = DIRECTION ( 'NONE',  ( -1.000000000000000000, 0.000000000000000000, 0.000000000000000000 ) ) ;
#12334 = LINE ( 'NONE', #11089, #2062 ) ;
#12335 = DIRECTION ( 'NONE',  ( -2.273843122241288438E-18, -5.551115123125783935E-17, -1.000000000000000000 ) ) ;
#12336 = ORIENTED_EDGE ( 'NONE', *, *, #11158, .T. ) ;
#12337 = VERTEX_POINT ( 'NONE', #5050 ) ;
#12338 = DIRECTION ( 'NONE',  ( 0.000000000000000000, -3.108624468950437130E-15, -1.000000000000000000 ) ) ;
#12339 = CARTESIAN_POINT ( 'NONE',  ( 3.974175853610007358, 2.726149789692824399, 2.409821656223152697 ) ) ;
#12340 = AXIS2_PLACEMENT_3D ( 'NONE', #4706, #10404, #165 ) ;
#12341 = AXIS2_PLACEMENT_3D ( 'NONE', #9092, #3348, #7786 ) ;
#12342 = AXIS2_PLACEMENT_3D ( 'NONE', #8306, #6921, #9266 ) ;
#12343 = ORIENTED_EDGE ( 'NONE', *, *, #12937, .F. ) ;
#12344 = EDGE_LOOP ( 'NONE', ( #2627, #9111, #2553, #14084 ) ) ;
#12345 = ORIENTED_EDGE ( 'NONE', *, *, #11829, .F. ) ;
#12346 = DIRECTION ( 'NONE',  ( 0.000000000000000000, 0.000000000000000000, -1.000000000000000000 ) ) ;
#12347 = ORIENTED_EDGE ( 'NONE', *, *, #12323, .T. ) ;
#12348 = FACE_OUTER_BOUND ( 'NONE', #3130, .T. ) ;
#12349 = DIRECTION ( 'NONE',  ( 0.000000000000000000, 0.000000000000000000, -1.000000000000000000 ) ) ;
#12350 = AXIS2_PLACEMENT_3D ( 'NONE', #3145, #14189, #10948 ) ;
#12351 = PLANE ( 'NONE',  #10037 ) ;
#12352 = DIRECTION ( 'NONE',  ( 3.469446951953791374E-18, -0.5000000000000012212, -0.8660254037844380415 ) ) ;
#12353 = AXIS2_PLACEMENT_3D ( 'NONE', #3489, #3563, #7997 ) ;
#12354 = ORIENTED_EDGE ( 'NONE', *, *, #11821, .T. ) ;
#12355 = CARTESIAN_POINT ( 'NONE',  ( 4.175813232069169878, 2.061359961916364725, 3.570380186727388327 ) ) ;
#12356 = CONTEXT_DEPENDENT_SHAPE_REPRESENTATION ( #8953, #10103 ) ;
#12357 = VECTOR ( 'NONE', #7631, 1000.000000000000000 ) ;
#12358 = CARTESIAN_POINT ( 'NONE',  ( 0.4022569922705621637, -5.541259509125479710, -0.4198507760575922454 ) ) ;
#12359 = CARTESIAN_POINT ( 'NONE',  ( 5.098157279263968000, -4.694029454718629424, -2.227990823963161669E-13 ) ) ;
#12360 =( BOUNDED_SURFACE ( )  B_SPLINE_SURFACE ( 3, 2, ( 
 ( #8464, #9338, #2928 ),
 ( #3795, #7424, #4380 ),
 ( #4315, #14118, #4238 ),
 ( #8676, #12191, #790 ),
 ( #11090, #13020, #9774 ),
 ( #2094, #2172, #8600 ) ),
 .UNSPECIFIED., .F., .F., .T. ) 
 B_SPLINE_SURFACE_WITH_KNOTS ( ( 4, 2, 4 ),
 ( 3, 3 ),
 ( 0.01651732063679902870, 0.01857756227444015348, 0.02063780391208127826 ),
 ( 0.000000000000000000, 1.000000000000000000 ),
 .UNSPECIFIED. ) 
 GEOMETRIC_REPRESENTATION_ITEM ( )  RATIONAL_B_SPLINE_SURFACE ( (
 ( 1.000000000000000000, 0.8047781231227495446, 1.000000000000000000),
 ( 1.000000000000000000, 0.8123782108664119317, 1.000000000000000000),
 ( 1.000000000000000000, 0.8190665102134654374, 1.000000000000000000),
 ( 1.000000000000000000, 0.8192358432842802296, 1.000000000000000000),
 ( 1.000000000000000000, 0.8126132624436200880, 1.000000000000000000),
 ( 1.000000000000000000, 0.8047712436238865230, 1.000000000000000000) ) ) 
 REPRESENTATION_ITEM ( '' )  SURFACE ( )  );
#12361 = FACE_OUTER_BOUND ( 'NONE', #3589, .T. ) ;
#12362 = EDGE_CURVE ( 'NONE', #9662, #5517, #4186, .T. ) ;
#12363 = ORIENTED_EDGE ( 'NONE', *, *, #1307, .T. ) ;
#12364 = VECTOR ( 'NONE', #2410, 1000.000000000000000 ) ;
#12365 = DIRECTION ( 'NONE',  ( -1.000000000000000000, 0.000000000000000000, 0.000000000000000000 ) ) ;
#12366 = ORIENTED_EDGE ( 'NONE', *, *, #12248, .F. ) ;
#12367 = SURFACE_SIDE_STYLE ('',( #11048 ) ) ;
#12368 = CARTESIAN_POINT ( 'NONE',  ( 20.00000000000000711, 20.00000000000000355, 25.00000000000000000 ) ) ;
#12369 = DIRECTION ( 'NONE',  ( -1.000000000000000000, 0.000000000000000000, 0.000000000000000000 ) ) ;
#12370 = FACE_OUTER_BOUND ( 'NONE', #4392, .T. ) ;
#12371 = DIRECTION ( 'NONE',  ( 0.000000000000000000, 1.000000000000000000, 0.000000000000000000 ) ) ;
#12372 = DIRECTION ( 'NONE',  ( -1.000000000000000000, 0.000000000000000000, 0.000000000000000000 ) ) ;
#12373 = EDGE_CURVE ( 'NONE', #11965, #13624, #3964, .T. ) ;
#12374 = DIRECTION ( 'NONE',  ( -1.000000000000000000, 0.000000000000000000, 0.000000000000000000 ) ) ;
#12375 = ORIENTED_EDGE ( 'NONE', *, *, #2085, .T. ) ;
#12376 = LINE ( 'NONE', #1253, #4425 ) ;
#12377 = CARTESIAN_POINT ( 'NONE',  ( 2.750000000000002665, 2.500000000000002220, 0.000000000000000000 ) ) ;
#12378 = VECTOR ( 'NONE', #5397, 1000.000000000000000 ) ;
#12379 = EDGE_CURVE ( 'NONE', #6291, #10652, #1914, .T. ) ;
#12380 = VERTEX_POINT ( 'NONE', #3090 ) ;
#12381 = ORIENTED_EDGE ( 'NONE', *, *, #6631, .T. ) ;
#12382 = CIRCLE ( 'NONE', #1389, 2.500000000000002220 ) ;
#12383 = CARTESIAN_POINT ( 'NONE',  ( 4.862831555537458605, -4.276542471545712765, 0.5928111585566232522 ) ) ;
#12384 = DIRECTION ( 'NONE',  ( 1.000000000000000000, 0.000000000000000000, 0.000000000000000000 ) ) ;
#12385 = DIRECTION ( 'NONE',  ( -0.000000000000000000, -1.000000000000000000, 0.000000000000000000 ) ) ;
#12386 = MECHANICAL_DESIGN_GEOMETRIC_PRESENTATION_REPRESENTATION (  '', ( #1384 ), #2566 ) ;
#12387 = ADVANCED_FACE ( 'NONE', ( #7518 ), #11326, .F. ) ;
#12388 = CARTESIAN_POINT ( 'NONE',  ( 5.103021810857296892, 2.353405741490996128, 4.076218315086678423 ) ) ;
#12389 = ORIENTED_EDGE ( 'NONE', *, *, #7441, .T. ) ;
#12390 = CARTESIAN_POINT ( 'NONE',  ( 4.872112557122744825, 2.415041619695410755E-11, 4.072377784234180176 ) ) ;
#12391 = VECTOR ( 'NONE', #9611, 1000.000000000000000 ) ;
#12392 = VERTEX_POINT ( 'NONE', #9046 ) ;
#12393 = DIRECTION ( 'NONE',  ( 0.000000000000000000, 0.000000000000000000, -1.000000000000000000 ) ) ;
#12394 = ADVANCED_FACE ( 'NONE', ( #10011 ), #7879, .T. ) ;
#12395 = DIRECTION ( 'NONE',  ( 0.000000000000000000, 0.000000000000000000, -1.000000000000000000 ) ) ;
#12396 = DIRECTION ( 'NONE',  ( 1.734723475976807094E-16, 0.000000000000000000, -1.000000000000000000 ) ) ;
#12397 = CARTESIAN_POINT ( 'NONE',  ( -2.500000000000000444, 3.775608651740452848E-15, -5.624496230895170257 ) ) ;
#12398 = AXIS2_PLACEMENT_3D ( 'NONE', #1663, #6112, #10594 ) ;
#12399 = FACE_OUTER_BOUND ( 'NONE', #4325, .T. ) ;
#12400 = AXIS2_PLACEMENT_3D ( 'NONE', #11073, #3403, #6743 ) ;
#12401 = CARTESIAN_POINT ( 'NONE',  ( 44.62907851819101523, 71.79144999128007498, 25.00000000000000000 ) ) ;
#12402 = EDGE_CURVE ( 'NONE', #3420, #12252, #50, .T. ) ;
#12403 = CARTESIAN_POINT ( 'NONE',  ( 39.77836601746437850, 91.19429999418670718, 25.00000000000000000 ) ) ;
#12404 = VECTOR ( 'NONE', #6593, 1000.000000000000000 ) ;
#12405 = ORIENTED_EDGE ( 'NONE', *, *, #2623, .F. ) ;
#12406 = EDGE_CURVE ( 'NONE', #8264, #4092, #4545, .T. ) ;
#12407 = DIRECTION ( 'NONE',  ( 0.000000000000000000, -1.000000000000000000, 0.000000000000000000 ) ) ;
#12408 = ORIENTED_EDGE ( 'NONE', *, *, #2222, .T. ) ;
#12409 = DIRECTION ( 'NONE',  ( -1.000000000000000000, 0.000000000000000000, 0.000000000000000000 ) ) ;
#12410 = AXIS2_PLACEMENT_3D ( 'NONE', #3518, #6872, #11981 ) ;
#12411 = CARTESIAN_POINT ( 'NONE',  ( 13.00000000000000355, 24.50000000000001421, 0.000000000000000000 ) ) ;
#12412 = AXIS2_PLACEMENT_3D ( 'NONE', #12150, #12018, #6577 ) ;
#12413 = CONICAL_SURFACE ( 'NONE', #5164, 2.450000000000000622, 0.9599310885968804774 ) ;
#12414 = ORIENTED_EDGE ( 'NONE', *, *, #12914, .T. ) ;
#12415 = ORIENTED_EDGE ( 'NONE', *, *, #11158, .F. ) ;
#12416 = EDGE_LOOP ( 'NONE', ( #6087, #11080, #7999, #9302 ) ) ;
#12417 = DIRECTION ( 'NONE',  ( -0.000000000000000000, -1.000000000000000000, 0.000000000000000000 ) ) ;
#12418 = ORIENTED_EDGE ( 'NONE', *, *, #13211, .T. ) ;
#12419 = CARTESIAN_POINT ( 'NONE',  ( 4.086262841041381932, 2.102637316508702447, -3.499999999999992450 ) ) ;
#12420 = DIRECTION ( 'NONE',  ( -0.2425356250363330524, 0.9701425001453318764, 0.000000000000000000 ) ) ;
#12421 = DIRECTION ( 'NONE',  ( 0.000000000000000000, 0.000000000000000000, 1.000000000000000000 ) ) ;
#12422 = VECTOR ( 'NONE', #5624, 1000.000000000000000 ) ;
#12423 = DIRECTION ( 'NONE',  ( 0.000000000000000000, 0.000000000000000000, 1.000000000000000000 ) ) ;
#12424 = MECHANICAL_DESIGN_GEOMETRIC_PRESENTATION_REPRESENTATION (  '', ( #4269 ), #9375 ) ;
#12425 = AXIS2_PLACEMENT_3D ( 'NONE', #7009, #2486, #8258 ) ;
#12426 = EDGE_CURVE ( 'NONE', #8706, #2703, #9112, .T. ) ;
#12427 = DIRECTION ( 'NONE',  ( 0.000000000000000000, 0.000000000000000000, 1.000000000000000000 ) ) ;
#12428 = CONTEXT_DEPENDENT_SHAPE_REPRESENTATION ( #1478, #13990 ) ;
#12429 = CARTESIAN_POINT ( 'NONE',  ( 3.951447005078475350, 3.704664227300108692, 0.5833333333333335924 ) ) ;
#12430 = CARTESIAN_POINT ( 'NONE',  ( 4.052424581287699112, -2.393186648133069916, 2.990837702970342349 ) ) ;
#12431 = ORIENTED_EDGE ( 'NONE', *, *, #13715, .T. ) ;
#12432 = VECTOR ( 'NONE', #12330, 1000.000000000000000 ) ;
#12433 = VECTOR ( 'NONE', #1231, 1000.000000000000000 ) ;
#12434 = TOROIDAL_SURFACE ( 'NONE', #1924, 3.199999999999998845, 0.8000000000000001554 ) ;
#12435 = EDGE_LOOP ( 'NONE', ( #378, #8080, #10147, #708 ) ) ;
#12436 = FACE_OUTER_BOUND ( 'NONE', #7563, .T. ) ;
#12437 = ORIENTED_EDGE ( 'NONE', *, *, #4059, .T. ) ;
#12438 = ORIENTED_EDGE ( 'NONE', *, *, #13458, .F. ) ;
#12439 = CARTESIAN_POINT ( 'NONE',  ( -24.99999999999998934, 199.5765550933606107, -2.000000000000001776 ) ) ;
#12440 = CARTESIAN_POINT ( 'NONE',  ( 28.00000000000000355, 29.99999999999999645, -34.50000000000000000 ) ) ;
#12441 = ORIENTED_EDGE ( 'NONE', *, *, #3346, .T. ) ;
#12442 = EDGE_CURVE ( 'NONE', #6626, #12702, #5610, .T. ) ;
#12443 = CARTESIAN_POINT ( 'NONE',  ( 22.00000000000000000, 80.00000000000000000, -25.00000000000000000 ) ) ;
#12444 = DIRECTION ( 'NONE',  ( -1.000000000000000000, 0.000000000000000000, 0.000000000000000000 ) ) ;
#12445 = ADVANCED_FACE ( 'NONE', ( #6640 ), #4400, .T. ) ;
#12446 =( GEOMETRIC_REPRESENTATION_CONTEXT ( 3 ) GLOBAL_UNCERTAINTY_ASSIGNED_CONTEXT ( ( #9534 ) ) GLOBAL_UNIT_ASSIGNED_CONTEXT ( ( #12320, #9078, #1122 ) ) REPRESENTATION_CONTEXT ( 'NONE', 'WORKASPACE' ) );
#12447 = DIRECTION ( 'NONE',  ( -0.000000000000000000, 8.482162385747133845E-47, -1.000000000000000000 ) ) ;
#12448 = ORIENTED_EDGE ( 'NONE', *, *, #11341, .F. ) ;
#12449 = VECTOR ( 'NONE', #4980, 1000.000000000000000 ) ;
#12450 = PRODUCT_DEFINITION_SHAPE ( 'NONE', 'NONE',  #14467 ) ;
#12451 = LINE ( 'NONE', #5828, #10102 ) ;
#12452 = ORIENTED_EDGE ( 'NONE', *, *, #4034, .T. ) ;
#12453 = EDGE_CURVE ( 'NONE', #14098, #313, #12215, .T. ) ;
#12454 = VECTOR ( 'NONE', #4155, 1000.000000000000000 ) ;
#12455 = LINE ( 'NONE', #228, #11859 ) ;
#12456 = CARTESIAN_POINT ( 'NONE',  ( 0.000000000000000000, 25.49999999999996803, 8.000000000000007105 ) ) ;
#12457 =( LENGTH_UNIT ( ) NAMED_UNIT ( * ) SI_UNIT ( .MILLI., .METRE. ) );
#12458 = EDGE_CURVE ( 'NONE', #8390, #5783, #70, .T. ) ;
#12459 = EDGE_CURVE ( 'NONE', #13816, #14126, #8072, .T. ) ;
#12460 = PLANE ( 'NONE',  #4634 ) ;
#12461 = CONICAL_SURFACE ( 'NONE', #6612, 4.000000000000000000, 0.8911886515913775009 ) ;
#12462 = CARTESIAN_POINT ( 'NONE',  ( -5.560781378645576645, -9.260561282218706512E-16, -3.699999999999981082 ) ) ;
#12463 = ADVANCED_FACE ( 'NONE', ( #9267 ), #8166, .T. ) ;
#12464 = DIRECTION ( 'NONE',  ( 1.000000000000000000, -4.625929269271486900E-16, -0.000000000000000000 ) ) ;
#12465 = B_SPLINE_CURVE_WITH_KNOTS ( 'NONE', 3,
 ( #10423, #4868, #1427, #5873, #4799, #3710, #640, #13736, #3860, #9329, #5020, #13813, #2685, #5084, #8294, #12768 ),
 .UNSPECIFIED., .F., .F.,
 ( 4, 3, 3, 3, 3, 4 ),
 ( 0.000000000000000000, 3.647308126642503462E-05, 7.269606878412154284E-05, 0.0001129253843484836974, 0.0001515766232005116496, 0.0001537911822990434198 ),
 .UNSPECIFIED. ) ;
#12466 = VECTOR ( 'NONE', #6789, 1000.000000000000000 ) ;
#12467 = ADVANCED_FACE ( 'NONE', ( #5964 ), #13752, .T. ) ;
#12468 = DIRECTION ( 'NONE',  ( -1.387778780781446415E-16, 0.000000000000000000, -1.000000000000000000 ) ) ;
#12469 = DIRECTION ( 'NONE',  ( 0.000000000000000000, 0.000000000000000000, -1.000000000000000000 ) ) ;
#12470 = AXIS2_PLACEMENT_3D ( 'NONE', #11478, #4760, #13917 ) ;
#12471 = CARTESIAN_POINT ( 'NONE',  ( 4.175572532730949860, -2.061029303918050282, -3.569807470274399375 ) ) ;
#12472 = DIRECTION ( 'NONE',  ( 0.000000000000000000, 0.000000000000000000, 1.000000000000000000 ) ) ;
#12473 = SURFACE_STYLE_FILL_AREA ( #325 ) ;
#12474 = FACE_OUTER_BOUND ( 'NONE', #11986, .T. ) ;
#12475 = CARTESIAN_POINT ( 'NONE',  ( -0.8441225671354688487, 5.568793373801097957, -4.476900509771803982 ) ) ;
#12476 = EDGE_LOOP ( 'NONE', ( #5704, #1149, #8873, #4111 ) ) ;
#12477 = CARTESIAN_POINT ( 'NONE',  ( 0.000000000000000000, 0.000000000000000000, -4.699999999999981526 ) ) ;
#12478 = AXIS2_PLACEMENT_3D ( 'NONE', #12329, #4646, #2301 ) ;
#12479 = EDGE_LOOP ( 'NONE', ( #2878, #7386 ) ) ;
#12480 = DIRECTION ( 'NONE',  ( 0.2425356250363327748, -0.9701425001453319874, -0.000000000000000000 ) ) ;
#12481 = ORIENTED_EDGE ( 'NONE', *, *, #8159, .F. ) ;
#12482 = CARTESIAN_POINT ( 'NONE',  ( 0.000000000000000000, 0.000000000000000000, 0.000000000000000000 ) ) ;
#12483 = VERTEX_POINT ( 'NONE', #8240 ) ;
#12484 = ORIENTED_EDGE ( 'NONE', *, *, #7161, .T. ) ;
#12485 = ADVANCED_FACE ( 'NONE', ( #1586 ), #10519, .F. ) ;
#12486 = ORIENTED_EDGE ( 'NONE', *, *, #8427, .T. ) ;
#12487 = CARTESIAN_POINT ( 'NONE',  ( 4.960471971868395613, -4.315143281044174550, -0.6753920894104464834 ) ) ;
#12488 = CLOSED_SHELL ( 'NONE', ( #2437, #702, #14077, #9003, #7116, #11352, #1765, #10028, #13693, #13118, #14334, #5592, #5116, #11841, #5805, #13473, #5708, #4009, #2662, #8309, #4433, #6000, #8825, #11357, #8338, #10481, #6289 ) ) ;
#12489 = ORIENTED_EDGE ( 'NONE', *, *, #9373, .T. ) ;
#12490 = CARTESIAN_POINT ( 'NONE',  ( 20.00000000000000000, -5.510910596163090344E-15, 25.00000000000000000 ) ) ;
#12491 = DIRECTION ( 'NONE',  ( -0.2425356250363330801, 0.9701425001453319874, 0.000000000000000000 ) ) ;
#12492 = CARTESIAN_POINT ( 'NONE',  ( 57.35294117647057277, -1.411764705882362358, 25.00000000000000000 ) ) ;
#12493 = DIRECTION ( 'NONE',  ( -3.286707217423840556E-17, -1.000000000000000000, -2.220446049250313574E-16 ) ) ;
#12494 = CARTESIAN_POINT ( 'NONE',  ( -28.00000000000000355, 29.99999999999999645, 8.000000000000007105 ) ) ;
#12495 = ITEM_DEFINED_TRANSFORMATION ( 'NONE', 'NONE', #7797,  #11025 ) ;
#12496 = DIRECTION ( 'NONE',  ( 1.000000000000000000, 1.665334536937734071E-16, 0.000000000000000000 ) ) ;
#12497 = CARTESIAN_POINT ( 'NONE',  ( 0.8333333333333322601, -5.292377467571611760, -4.118275046351174140 ) ) ;
#12498 = PLANE ( 'NONE',  #7744 ) ;
#12499 = EDGE_CURVE ( 'NONE', #4722, #9673, #10222, .T. ) ;
#12500 = PRODUCT_DEFINITION ( 'UNKNOWN', '', #1023, #6739 ) ;
#12501 = EDGE_CURVE ( 'NONE', #5269, #9564, #3725, .T. ) ;
#12502 = ORIENTED_EDGE ( 'NONE', *, *, #4368, .F. ) ;
#12503 = CARTESIAN_POINT ( 'NONE',  ( -0.5469803261939266692, 4.303002914946603141, -3.235259548912158944 ) ) ;
#12504 = ORIENTED_EDGE ( 'NONE', *, *, #11015, .T. ) ;
#12505 = FACE_BOUND ( 'NONE', #8985, .T. ) ;
#12506 = CARTESIAN_POINT ( 'NONE',  ( 4.960411150172102879, 1.572332708191227058, -4.074718599813436093 ) ) ;
#12507 = CARTESIAN_POINT ( 'NONE',  ( 0.000000000000000000, 0.000000000000000000, 0.000000000000000000 ) ) ;
#12508 = DIRECTION ( 'NONE',  ( 1.000000000000000000, 0.000000000000000000, 0.000000000000000000 ) ) ;
#12509 = ORIENTED_EDGE ( 'NONE', *, *, #3686, .T. ) ;
#12510 = CARTESIAN_POINT ( 'NONE',  ( 51.83050351964435976, 32.98574998546678927, 25.00000000000000000 ) ) ;
#12511 = DIRECTION ( 'NONE',  ( 0.000000000000000000, -0.000000000000000000, -1.000000000000000000 ) ) ;
#12512 = LINE ( 'NONE', #10241, #1930 ) ;
#12513 = VERTEX_POINT ( 'NONE', #11324 ) ;
#12514 = ORIENTED_EDGE ( 'NONE', *, *, #7683, .F. ) ;
#12515 = CARTESIAN_POINT ( 'NONE',  ( -3.355112389629170355, 2.681727112203163621, -0.2256878752776750874 ) ) ;
#12516 = CARTESIAN_POINT ( 'NONE',  ( 20.00000000000000000, 37.00000000000000711, 25.00000000000000000 ) ) ;
#12517 =( BOUNDED_SURFACE ( )  B_SPLINE_SURFACE ( 3, 2, ( 
 ( #6721, #8989, #6933 ),
 ( #8100, #1166, #84 ),
 ( #1458, #1375, #13628 ),
 ( #4687, #8175, #4617 ),
 ( #5690, #8034, #5902 ),
 ( #10233, #13549, #10386 ) ),
 .UNSPECIFIED., .F., .F., .T. ) 
 B_SPLINE_SURFACE_WITH_KNOTS ( ( 4, 2, 4 ),
 ( 3, 3 ),
 ( 0.02462896261017847102, 0.02769666342207012522, 0.03076436423396178288 ),
 ( 0.000000000000000000, 1.000000000000000000 ),
 .UNSPECIFIED. ) 
 GEOMETRIC_REPRESENTATION_ITEM ( )  RATIONAL_B_SPLINE_SURFACE ( (
 ( 1.000000000000000000, 0.8047780983185548465, 1.000000000000000000),
 ( 1.000000000000000000, 0.8123789199823617801, 1.000000000000000000),
 ( 1.000000000000000000, 0.8190678250840702779, 1.000000000000000000),
 ( 1.000000000000000000, 0.8192345812593594401, 1.000000000000000000),
 ( 1.000000000000000000, 0.8126126716515976733, 1.000000000000000000),
 ( 1.000000000000000000, 0.8047712641343244266, 1.000000000000000000) ) ) 
 REPRESENTATION_ITEM ( '' )  SURFACE ( )  );
#12518 = EDGE_CURVE ( 'NONE', #11932, #10034, #6347, .T. ) ;
#12519 = VERTEX_POINT ( 'NONE', #13616 ) ;
#12520 = ORIENTED_EDGE ( 'NONE', *, *, #11967, .T. ) ;
#12521 = FACE_OUTER_BOUND ( 'NONE', #1036, .T. ) ;
#12522 = DIRECTION ( 'NONE',  ( -1.000000000000000000, 0.000000000000000000, 0.000000000000000000 ) ) ;
#12523 = ORIENTED_EDGE ( 'NONE', *, *, #2016, .F. ) ;
#12524 = DIRECTION ( 'NONE',  ( -1.000000000000000000, 0.000000000000000000, 0.000000000000000000 ) ) ;
#12525 = EDGE_CURVE ( 'NONE', #7201, #12696, #3654, .T. ) ;
#12526 = EDGE_CURVE ( 'NONE', #8584, #6205, #11260, .T. ) ;
#12527 = CARTESIAN_POINT ( 'NONE',  ( 20.00000000000000000, 47.00000000000000000, 25.00000000000000000 ) ) ;
#12528 = LINE ( 'NONE', #543, #12004 ) ;
#12529 = DIRECTION ( 'NONE',  ( -3.469446951953772885E-18, -7.771561172376088880E-16, 1.000000000000000000 ) ) ;
#12530 = DIRECTION ( 'NONE',  ( 0.000000000000000000, 0.000000000000000000, -1.000000000000000000 ) ) ;
#12531 = VECTOR ( 'NONE', #19, 999.9999999999998863 ) ;
#12532 = SURFACE_STYLE_USAGE ( .BOTH. , #4719 ) ;
#12533 = CARTESIAN_POINT ( 'NONE',  ( 3.806834918298616088, 3.031088913245548966, -1.750000000000005551 ) ) ;
#12534 = CARTESIAN_POINT ( 'NONE',  ( -0.7030283904642582460, 5.367609061415551608, -4.396693167835974414 ) ) ;
#12535 = VERTEX_POINT ( 'NONE', #7065 ) ;
#12536 = CARTESIAN_POINT ( 'NONE',  ( 42.12907851819100813, 71.79144999128007498, 25.00000000000000000 ) ) ;
#12537 = ORIENTED_EDGE ( 'NONE', *, *, #8079, .F. ) ;
#12538 = CARTESIAN_POINT ( 'NONE',  ( 0.000000000000000000, 249.5765550933606391, 4.000000000000003553 ) ) ;
#12539 = EDGE_CURVE ( 'NONE', #9023, #6870, #14377, .T. ) ;
#12540 = DIRECTION ( 'NONE',  ( 0.000000000000000000, 1.000000000000000000, -0.000000000000000000 ) ) ;
#12541 = VERTEX_POINT ( 'NONE', #3803 ) ;
#12542 = CARTESIAN_POINT ( 'NONE',  ( 0.000000000000000000, 0.000000000000000000, 23.00000000000000000 ) ) ;
#12544 = ORIENTED_EDGE ( 'NONE', *, *, #3685, .F. ) ;
#12543 = ADVANCED_FACE ( 'NONE', ( #4675 ), #3587, .F. ) ;
#12545 = DIRECTION ( 'NONE',  ( 0.000000000000000000, 8.482162385747133845E-47, -1.000000000000000000 ) ) ;
#12546 = CIRCLE ( 'NONE', #10909, 4.750000000000000000 ) ;
#12547 = VERTEX_POINT ( 'NONE', #4881 ) ;
#12548 = CYLINDRICAL_SURFACE ( 'NONE', #11308, 2.750000000000003553 ) ;
#12549 = DIRECTION ( 'NONE',  ( -1.000000000000000000, 0.000000000000000000, 0.000000000000000000 ) ) ;
#12550 = ORIENTED_EDGE ( 'NONE', *, *, #2030, .T. ) ;
#12551 = DIRECTION ( 'NONE',  ( 0.000000000000000000, 0.000000000000000000, 1.000000000000000000 ) ) ;
#12552 = PRODUCT ( 'BR-599', 'BR-599', '', ( #9874 ) ) ;
#12553 = DIRECTION ( 'NONE',  ( 0.000000000000000000, 0.000000000000000000, 1.000000000000000000 ) ) ;
#12554 = DIRECTION ( 'NONE',  ( 1.000000000000000000, 0.000000000000000000, 0.000000000000000000 ) ) ;
#12555 = DIRECTION ( 'NONE',  ( 0.2425356250363327748, -0.9701425001453319874, -0.000000000000000000 ) ) ;
#12556 = CARTESIAN_POINT ( 'NONE',  ( 19.99999999999999645, 67.00000000000000000, 25.00000000000000000 ) ) ;
#12557 = ITEM_DEFINED_TRANSFORMATION ( 'NONE', 'NONE', #1491,  #11025 ) ;
#12558 = DIRECTION ( 'NONE',  ( 1.000000000000000000, 0.000000000000000000, -0.000000000000000000 ) ) ;
#12559 = VECTOR ( 'NONE', #7843, 999.9999999999998863 ) ;
#12560 = CARTESIAN_POINT ( 'NONE',  ( 4.872112557122744825, 2.415041619695410755E-11, 4.072377784234180176 ) ) ;
#12561 = ADVANCED_FACE ( 'NONE', ( #9343 ), #12498, .T. ) ;
#12562 = DIRECTION ( 'NONE',  ( 0.000000000000000000, 0.000000000000000000, -1.000000000000000000 ) ) ;
#12563 = VECTOR ( 'NONE', #12710, 1000.000000000000000 ) ;
#12564 = VERTEX_POINT ( 'NONE', #11610 ) ;
#12565 = DIRECTION ( 'NONE',  ( 0.000000000000000000, 0.000000000000000000, -1.000000000000000000 ) ) ;
#12566 = VECTOR ( 'NONE', #9529, 1000.000000000000114 ) ;
#12567 = EDGE_LOOP ( 'NONE', ( #13156, #13117, #13948, #8807 ) ) ;
#12568 = VECTOR ( 'NONE', #7112, 1000.000000000000000 ) ;
#12569 = FACE_OUTER_BOUND ( 'NONE', #9560, .T. ) ;
#12570 = LINE ( 'NONE', #5901, #10998 ) ;
#12571 = SURFACE_STYLE_USAGE ( .BOTH. , #3664 ) ;
#12572 = LINE ( 'NONE', #4618, #2837 ) ;
#12573 = ORIENTED_EDGE ( 'NONE', *, *, #293, .F. ) ;
#12574 = CARTESIAN_POINT ( 'NONE',  ( 0.000000000000000000, 3.031088913245522320, 1.750000000000001554 ) ) ;
#12575 = ADVANCED_FACE ( 'NONE', ( #3872 ), #4959, .T. ) ;
#12576 = DIRECTION ( 'NONE',  ( -1.000000000000000000, 0.000000000000000000, 0.000000000000000000 ) ) ;
#12577 = EDGE_CURVE ( 'NONE', #6929, #9740, #2474, .T. ) ;
#12578 = ORIENTED_EDGE ( 'NONE', *, *, #12896, .F. ) ;
#12579 = AXIS2_PLACEMENT_3D ( 'NONE', #4482, #212, #13252 ) ;
#12580 = CARTESIAN_POINT ( 'NONE',  ( 20.00000000000000000, 70.00000000000000000, -25.00000000000000000 ) ) ;
#12581 = VERTEX_POINT ( 'NONE', #12866 ) ;
#12582 = ORIENTED_EDGE ( 'NONE', *, *, #3829, .T. ) ;
#12583 = LINE ( 'NONE', #12658, #3677 ) ;
#12584 = DIRECTION ( 'NONE',  ( 1.000000000000000000, 0.000000000000000000, 0.000000000000000000 ) ) ;
#12585 = ORIENTED_EDGE ( 'NONE', *, *, #3027, .F. ) ;
#12586 = EDGE_CURVE ( 'NONE', #4153, #4403, #7215, .T. ) ;
#12587 = VECTOR ( 'NONE', #7510, 1000.000000000000000 ) ;
#12588 = ORIENTED_EDGE ( 'NONE', *, *, #11540, .F. ) ;
#12589 = CARTESIAN_POINT ( 'NONE',  ( 53.99999999999997868, -1.324077043022348342E-15, -23.00000000000000000 ) ) ;
#12590 = DIRECTION ( 'NONE',  ( 0.000000000000000000, 0.000000000000000000, 1.000000000000000000 ) ) ;
#12591 = ORIENTED_EDGE ( 'NONE', *, *, #7298, .T. ) ;
#12592 = CYLINDRICAL_SURFACE ( 'NONE', #554, 2.500000000000002220 ) ;
#12593 = VECTOR ( 'NONE', #6556, 1000.000000000000000 ) ;
#12594 = UNCERTAINTY_MEASURE_WITH_UNIT (LENGTH_MEASURE( 1.000000000000000082E-05 ), #1937, 'distance_accuracy_value', 'NONE');
#12595 = DIRECTION ( 'NONE',  ( 0.000000000000000000, 1.000000000000000000, 0.000000000000000000 ) ) ;
#12596 = CARTESIAN_POINT ( 'NONE',  ( 4.132952817037849336, 2.031684012687246188, 3.518979934899739259 ) ) ;
#12597 = ORIENTED_EDGE ( 'NONE', *, *, #14316, .F. ) ;
#12598 = CARTESIAN_POINT ( 'NONE',  ( -2.500000000000016875, -4.330127018922186544, 0.000000000000000000 ) ) ;
#12599 = DIRECTION ( 'NONE',  ( -1.000000000000000000, 0.000000000000000000, 0.000000000000000000 ) ) ;
#12600 = B_SPLINE_CURVE_WITH_KNOTS ( 'NONE', 3,
 ( #9278, #11183, #1162, #12717, #7219, #11616 ),
 .UNSPECIFIED., .F., .F.,
 ( 4, 2, 4 ),
 ( 0.003358874760055545385, 0.004541967308452085975, 0.005725059856848626130 ),
 .UNSPECIFIED. ) ;
#12601 = LINE ( 'NONE', #2671, #5983 ) ;
#12602 = DIRECTION ( 'NONE',  ( 0.000000000000000000, 0.000000000000000000, -1.000000000000000000 ) ) ;
#12603 = ORIENTED_EDGE ( 'NONE', *, *, #13199, .T. ) ;
#12604 = DIRECTION ( 'NONE',  ( 0.000000000000000000, -8.482162385747133845E-47, 1.000000000000000000 ) ) ;
#12605 = VECTOR ( 'NONE', #1527, 1000.000000000000114 ) ;
#12606 = ADVANCED_FACE ( 'NONE', ( #6116, #1667, #8387 ), #582, .T. ) ;
#12607 = DIRECTION ( 'NONE',  ( 1.000000000000000000, 1.665334536937734071E-16, 0.000000000000000000 ) ) ;
#12608 = FACE_OUTER_BOUND ( 'NONE', #4372, .T. ) ;
#12609 = ORIENTED_EDGE ( 'NONE', *, *, #2258, .T. ) ;
#12610 = CARTESIAN_POINT ( 'NONE',  ( -129.3408537872145132, 189.5765550933606107, -75.00000000000001421 ) ) ;
#12611 = FACE_BOUND ( 'NONE', #9083, .T. ) ;
#12612 = ORIENTED_EDGE ( 'NONE', *, *, #5959, .F. ) ;
#12613 = DIRECTION ( 'NONE',  ( -3.286707217423839940E-17, 1.000000000000000000, 6.695352868347748137E-17 ) ) ;
#12614 = EDGE_LOOP ( 'NONE', ( #12745, #8288, #14420, #13514, #13056 ) ) ;
#12615 = AXIS2_PLACEMENT_3D ( 'NONE', #7494, #11987, #1963 ) ;
#12616 = ORIENTED_EDGE ( 'NONE', *, *, #11754, .T. ) ;
#12617 = VECTOR ( 'NONE', #12551, 1000.000000000000000 ) ;
#12618 = DIRECTION ( 'NONE',  ( -0.000000000000000000, -0.000000000000000000, -1.000000000000000000 ) ) ;
#12619 = CARTESIAN_POINT ( 'NONE',  ( -1.790396195872466123, 48.30096731618026951, 7.586517658982195655 ) ) ;
#12620 = EDGE_CURVE ( 'NONE', #13071, #12337, #5185, .T. ) ;
#12621 = DIRECTION ( 'NONE',  ( 0.000000000000000000, -8.482162385747133845E-47, 1.000000000000000000 ) ) ;
#12622 = LINE ( 'NONE', #11532, #3919 ) ;
#12623 = LINE ( 'NONE', #4808, #4878 ) ;
#12624 = DIRECTION ( 'NONE',  ( 0.000000000000000000, 0.000000000000000000, -1.000000000000000000 ) ) ;
#12625 = CARTESIAN_POINT ( 'NONE',  ( 27.30499999999998195, 3.061616997868382648E-16, -2.499999999999999556 ) ) ;
#12626 = EDGE_CURVE ( 'NONE', #1525, #1016, #10974, .T. ) ;
#12627 = CARTESIAN_POINT ( 'NONE',  ( 20.00000000000000355, 17.00000000000000000, 25.00000000000000000 ) ) ;
#12628 = DIRECTION ( 'NONE',  ( 0.000000000000000000, 0.000000000000000000, 1.000000000000000000 ) ) ;
#12629 = DIRECTION ( 'NONE',  ( 0.000000000000000000, 0.000000000000000000, 1.000000000000000000 ) ) ;
#12630 = VECTOR ( 'NONE', #255, 1000.000000000000000 ) ;
#12631 = CARTESIAN_POINT ( 'NONE',  ( 0.000000000000000000, 0.000000000000000000, -25.03750572909319061 ) ) ;
#12632 = AXIS2_PLACEMENT_3D ( 'NONE', #3688, #10559, #12831 ) ;
#12633 = EDGE_LOOP ( 'NONE', ( #9717, #8349, #4195, #11453, #1841 ) ) ;
#12634 = DIRECTION ( 'NONE',  ( 0.000000000000000000, 0.000000000000000000, -1.000000000000000000 ) ) ;
#12635 = ORIENTED_EDGE ( 'NONE', *, *, #7522, .F. ) ;
#12636 = ADVANCED_FACE ( 'NONE', ( #6802 ), #5627, .F. ) ;
#12637 = AXIS2_PLACEMENT_3D ( 'NONE', #11699, #10611, #596 ) ;
#12638 = EDGE_LOOP ( 'NONE', ( #3234, #12481, #10379 ) ) ;
#12639 = FACE_BOUND ( 'NONE', #3571, .T. ) ;
#12640 = COLOUR_RGB ( '', 0.31764706, 0.68627451, 0.89019608) ;
#12641 = CIRCLE ( 'NONE', #13371, 5.000000000000018652 ) ;
#12642 = LINE ( 'NONE', #1457, #9646 ) ;
#12643 = DIRECTION ( 'NONE',  ( 0.000000000000000000, 0.000000000000000000, 1.000000000000000000 ) ) ;
#12644 = B_SPLINE_CURVE_WITH_KNOTS ( 'NONE', 3,
 ( #9606, #13138, #624, #7334, #822, #11884 ),
 .UNSPECIFIED., .F., .F.,
 ( 4, 2, 4 ),
 ( 0.002044882221487529742, 0.003063384235218501520, 0.004081886248949473731 ),
 .UNSPECIFIED. ) ;
#12645 = DIRECTION ( 'NONE',  ( 0.000000000000000000, 0.000000000000000000, -1.000000000000000000 ) ) ;
#12646 = DIRECTION ( 'NONE',  ( -1.913084959030911013E-15, 1.000000000000000000, 0.000000000000000000 ) ) ;
#12647 = DIRECTION ( 'NONE',  ( -2.081668171172169006E-16, -0.000000000000000000, 1.000000000000000000 ) ) ;
#12648 = CARTESIAN_POINT ( 'NONE',  ( 0.000000000000000000, 0.000000000000000000, -25.00000000000000000 ) ) ;
#12649 = CARTESIAN_POINT ( 'NONE',  ( 5.076540720129295359, 2.330508241952952808, 4.036558682520539065 ) ) ;
#12650 = FACE_OUTER_BOUND ( 'NONE', #4885, .T. ) ;
#12651 = ORIENTED_EDGE ( 'NONE', *, *, #11297, .T. ) ;
#12652 = CIRCLE ( 'NONE', #9625, 3.000000000000001332 ) ;
#12653 = AXIS2_PLACEMENT_3D ( 'NONE', #8441, #12924, #7342 ) ;
#12654 = DIRECTION ( 'NONE',  ( -0.7071067811865513475, -2.272424659682189540E-16, -0.7071067811865437980 ) ) ;
#12655 = EDGE_LOOP ( 'NONE', ( #7779, #291, #12588, #8499, #14086 ) ) ;
#12656 = ADVANCED_FACE ( 'NONE', ( #12233 ), #8781, .T. ) ;
#12657 = ORIENTED_EDGE ( 'NONE', *, *, #9421, .F. ) ;
#12658 = CARTESIAN_POINT ( 'NONE',  ( 0.000000000000000000, 189.5765550933606107, 33.00000000000002842 ) ) ;
#12659 = CYLINDRICAL_SURFACE ( 'NONE', #12894, 2.750000000000003997 ) ;
#12660 =( GEOMETRIC_REPRESENTATION_CONTEXT ( 3 ) GLOBAL_UNCERTAINTY_ASSIGNED_CONTEXT ( ( #9087 ) ) GLOBAL_UNIT_ASSIGNED_CONTEXT ( ( #2368, #108, #9909 ) ) REPRESENTATION_CONTEXT ( 'NONE', 'WORKASPACE' ) );
#12661 = VECTOR ( 'NONE', #222, 1000.000000000000000 ) ;
#12662 = FILL_AREA_STYLE_COLOUR ( '', #6097 ) ;
#12663 = EDGE_LOOP ( 'NONE', ( #8928, #841, #9608 ) ) ;
#12664 = ORIENTED_EDGE ( 'NONE', *, *, #556, .F. ) ;
#12665 = CARTESIAN_POINT ( 'NONE',  ( -4.197393957002300446, -7.772664289393031077E-14, -3.203767560748911780 ) ) ;
#12666 = CARTESIAN_POINT ( 'NONE',  ( 59.10657227073432551, 3.881474981106830313, 25.00000000000000000 ) ) ;
#12667 = ORIENTED_EDGE ( 'NONE', *, *, #7934, .T. ) ;
#12668 = COLOUR_RGB ( '', 0.66274510, 0.83137255, 0.94901961) ;
#12669 = CARTESIAN_POINT ( 'NONE',  ( -5.122335214190881558, -2.957381614792619740, -4.581769937709098350 ) ) ;
#12670 = VECTOR ( 'NONE', #13788, 1000.000000000000000 ) ;
#12671 = VECTOR ( 'NONE', #6650, 1000.000000000000000 ) ;
#12672 = PRODUCT ( 'High-Tension Retraction Spring', 'High-Tension Retraction Spring', '', ( #6281 ) ) ;
#12673 = EDGE_CURVE ( 'NONE', #13416, #13043, #11270, .T. ) ;
#12674 = ADVANCED_FACE ( 'NONE', ( #5693 ), #7753, .F. ) ;
#12675 = CARTESIAN_POINT ( 'NONE',  ( 5.253368672218638125, 3.033033817057769532, -4.659491423763650886 ) ) ;
#12676 = CARTESIAN_POINT ( 'NONE',  ( 4.104070371397483541, 2.023683613428362005, 3.505122836902505146 ) ) ;
#12677 = ORIENTED_EDGE ( 'NONE', *, *, #10724, .T. ) ;
#12678 = CARTESIAN_POINT ( 'NONE',  ( 6.800000000000028244, 2.309401076758504701, -4.000000000000003553 ) ) ;
#12679 = FACE_BOUND ( 'NONE', #14449, .T. ) ;
#12680 = CARTESIAN_POINT ( 'NONE',  ( 0.8441225671342533765, 5.568793373800017932, -4.476900509771413184 ) ) ;
#12681 = CYLINDRICAL_SURFACE ( 'NONE', #6019, 5.499999999999975131 ) ;
#12682 = EDGE_CURVE ( 'NONE', #2216, #13588, #7199, .T. ) ;
#12683 = VECTOR ( 'NONE', #9399, 1000.000000000000000 ) ;
#12684 = EDGE_LOOP ( 'NONE', ( #2104, #10495, #6956, #10018 ) ) ;
#12685 = LINE ( 'NONE', #11230, #11712 ) ;
#12686 = ORIENTED_EDGE ( 'NONE', *, *, #109, .T. ) ;
#12687 = LINE ( 'NONE', #7115, #11416 ) ;
#12688 = CARTESIAN_POINT ( 'NONE',  ( 1.274241539467095841, 3.883118457693076397, -2.920601398289139006 ) ) ;
#12689 = VECTOR ( 'NONE', #13308, 1000.000000000000000 ) ;
#12690 = EDGE_LOOP ( 'NONE', ( #3332, #11210, #1452, #2938 ) ) ;
#12691 = DIRECTION ( 'NONE',  ( 0.000000000000000000, 0.000000000000000000, -1.000000000000000000 ) ) ;
#12692 = CARTESIAN_POINT ( 'NONE',  ( 21.68170757442808849, 141.2731697022877313, 23.00000000000000000 ) ) ;
#12693 = EDGE_LOOP ( 'NONE', ( #12275, #551, #2921, #845 ) ) ;
#12694 = PRODUCT_DEFINITION_FORMATION_WITH_SPECIFIED_SOURCE ( 'ANY', '', #12552, .NOT_KNOWN. ) ;
#12695 = LINE ( 'NONE', #485, #10778 ) ;
#12696 = VERTEX_POINT ( 'NONE', #5489 ) ;
#12697 = VERTEX_POINT ( 'NONE', #11191 ) ;
#12698 = ADVANCED_FACE ( 'NONE', ( #6503 ), #1172, .F. ) ;
#12699 = ORIENTED_EDGE ( 'NONE', *, *, #5105, .T. ) ;
#12700 = LINE ( 'NONE', #9562, #11079 ) ;
#12701 = CARTESIAN_POINT ( 'NONE',  ( 18.68170757442808849, 141.2731697022877313, 35.00000000000000000 ) ) ;
#12702 = VERTEX_POINT ( 'NONE', #12443 ) ;
#12703 = FACE_OUTER_BOUND ( 'NONE', #5658, .T. ) ;
#12704 = VECTOR ( 'NONE', #12395, 1000.000000000000000 ) ;
#12705 = CARTESIAN_POINT ( 'NONE',  ( -2.499999999999995115, -4.330127018922216742, -3.920524600599868403 ) ) ;
#12706 = LINE ( 'NONE', #575, #8607 ) ;
#12707 = FILL_AREA_STYLE_COLOUR ( '', #10992 ) ;
#12708 = CONTEXT_DEPENDENT_SHAPE_REPRESENTATION ( #1285, #4187 ) ;
#12709 = DIRECTION ( 'NONE',  ( -1.000000000000000000, 0.000000000000000000, 0.000000000000000000 ) ) ;
#12710 = DIRECTION ( 'NONE',  ( 0.000000000000000000, 0.000000000000000000, -1.000000000000000000 ) ) ;
#12711 = DIRECTION ( 'NONE',  ( -1.000000000000000000, 2.551526159633733968E-19, 1.987661601597216239E-18 ) ) ;
#12712 = CARTESIAN_POINT ( 'NONE',  ( 0.000000000000000000, 4.618802153517016507, -3.133295621305376422 ) ) ;
#12713 = ADVANCED_FACE ( 'NONE', ( #153 ), #4621, .T. ) ;
#12714 = AXIS2_PLACEMENT_3D ( 'NONE', #8277, #1553, #6002 ) ;
#12715 = ORIENTED_EDGE ( 'NONE', *, *, #9346, .T. ) ;
#12716 = EDGE_CURVE ( 'NONE', #12827, #13075, #9062, .T. ) ;
#12717 = CARTESIAN_POINT ( 'NONE',  ( 4.000000000000004441, -0.7890432684750890990, -0.04868663549882738112 ) ) ;
#12718 = ADVANCED_FACE ( 'NONE', ( #5296 ), #7554, .F. ) ;
#12719 = ORIENTED_EDGE ( 'NONE', *, *, #9346, .F. ) ;
#12720 = EDGE_CURVE ( 'NONE', #13907, #5618, #3236, .T. ) ;
#12721 = ORIENTED_EDGE ( 'NONE', *, *, #2187, .F. ) ;
#12722 = CARTESIAN_POINT ( 'NONE',  ( -140.0000000000003411, 189.5765550933606107, 47.99999999999998579 ) ) ;
#12723 = PLANE ( 'NONE',  #9833 ) ;
#12724 = CARTESIAN_POINT ( 'NONE',  ( 20.00000000000000000, -5.510910596163090344E-15, 25.00000000000000000 ) ) ;
#12725 = CARTESIAN_POINT ( 'NONE',  ( -1.387778780781445676E-14, -4.618802153517016507, -0.5000000000000004441 ) ) ;
#12726 = CARTESIAN_POINT ( 'NONE',  ( 5.103021810857252483, -2.353405741491008119, -4.076218315086701516 ) ) ;
#12727 = CARTESIAN_POINT ( 'NONE',  ( 20.00000000000000000, 27.00000000000000355, 25.00000000000000000 ) ) ;
#12728 = DIRECTION ( 'NONE',  ( 0.000000000000000000, 0.000000000000000000, -1.000000000000000000 ) ) ;
#12729 = CLOSED_SHELL ( 'NONE', ( #867, #4874, #11771, #1355, #5751, #12718, #12543, #1086, #12656, #3159, #6539, #6357, #995, #11105, #8976, #8541, #9084, #8438, #2029, #2525, #1642, #2441, #11641, #12895, #7847, #1921, #2427, #9552, #2857, #10756, #6159, #10187 ) ) ;
#12730 = DIRECTION ( 'NONE',  ( 0.000000000000000000, 0.000000000000000000, -1.000000000000000000 ) ) ;
#12731 = CARTESIAN_POINT ( 'NONE',  ( -118.6817075744279748, -20.42344490663959178, -117.0000000000000000 ) ) ;
#12732 = EDGE_CURVE ( 'NONE', #2625, #981, #89, .T. ) ;
#12733 = LINE ( 'NONE', #8109, #5883 ) ;
#12734 = ORIENTED_EDGE ( 'NONE', *, *, #11689, .T. ) ;
#12735 = EDGE_LOOP ( 'NONE', ( #4137, #5817, #14274, #4665, #8986 ) ) ;
#12736 = ORIENTED_EDGE ( 'NONE', *, *, #898, .T. ) ;
#12737 = ORIENTED_EDGE ( 'NONE', *, *, #2926, .F. ) ;
#12738 = LINE ( 'NONE', #7018, #2473 ) ;
#12739 = CARTESIAN_POINT ( 'NONE',  ( 20.00000000000000355, 30.00000000000000711, -25.00000000000000000 ) ) ;
#12740 = EDGE_LOOP ( 'NONE', ( #2661, #12328, #3605, #3758, #6272 ) ) ;
#12741 = ORIENTED_EDGE ( 'NONE', *, *, #10484, .T. ) ;
#12742 = CARTESIAN_POINT ( 'NONE',  ( 4.211140560182194292, -2.431303136016548017, -3.445885042887453231 ) ) ;
#12743 = EDGE_CURVE ( 'NONE', #11427, #7617, #12652, .T. ) ;
#12744 = CARTESIAN_POINT ( 'NONE',  ( 5.091953023115925347, 2.341213539480247352, -4.055100801747951067 ) ) ;
#12745 = ORIENTED_EDGE ( 'NONE', *, *, #10760, .T. ) ;
#12746 = LINE ( 'NONE', #1401, #11774 ) ;
#12747 = B_SPLINE_CURVE_WITH_KNOTS ( 'NONE', 3,
 ( #8526, #1948, #14174, #11901, #12042 ),
 .UNSPECIFIED., .F., .F.,
 ( 4, 1, 4 ),
 ( 0.000000000000000000, 0.002309401076758495382, 0.004618802153516990763 ),
 .UNSPECIFIED. ) ;
#12748 = UNCERTAINTY_MEASURE_WITH_UNIT (LENGTH_MEASURE( 1.000000000000000082E-05 ), #1791, 'distance_accuracy_value', 'NONE');
#12749 = EDGE_CURVE ( 'NONE', #2684, #8560, #4490, .T. ) ;
#12750 = CARTESIAN_POINT ( 'NONE',  ( -1.317756351988340180, 3.857995168970207889, -0.04852650426602111294 ) ) ;
#12751 = DIRECTION ( 'NONE',  ( -1.000000000000000000, 0.000000000000000000, 0.000000000000000000 ) ) ;
#12752 = CARTESIAN_POINT ( 'NONE',  ( 3.370256023960729782E-15, 5.773502691896274186, -6.000000000000005329 ) ) ;
#12753 = LINE ( 'NONE', #1789, #12391 ) ;
#12754 = FACE_BOUND ( 'NONE', #2335, .T. ) ;
#12755 =( NAMED_UNIT ( * ) PLANE_ANGLE_UNIT ( ) SI_UNIT ( $, .RADIAN. ) );
#12756 = VERTEX_POINT ( 'NONE', #3389 ) ;
#12757 = DIRECTION ( 'NONE',  ( 0.000000000000000000, 0.000000000000000000, -1.000000000000000000 ) ) ;
#12758 = DIRECTION ( 'NONE',  ( 2.312964634635743943E-16, -1.000000000000000000, -0.000000000000000000 ) ) ;
#12759 = ORIENTED_EDGE ( 'NONE', *, *, #5392, .F. ) ;
#12760 =( NAMED_UNIT ( * ) SI_UNIT ( $, .STERADIAN. ) SOLID_ANGLE_UNIT ( ) );
#12761 = LINE ( 'NONE', #4150, #871 ) ;
#12762 = ADVANCED_FACE ( 'NONE', ( #12302 ), #5417, .F. ) ;
#12763 = ADVANCED_FACE ( 'NONE', ( #4347, #2502, #5777 ), #9230, .F. ) ;
#12764 = FACE_OUTER_BOUND ( 'NONE', #9825, .T. ) ;
#12765 = ORIENTED_EDGE ( 'NONE', *, *, #5991, .F. ) ;
#12766 = CARTESIAN_POINT ( 'NONE',  ( 4.859329672867314542, -4.267091032106372417, -0.6091815318702474835 ) ) ;
#12767 = DIRECTION ( 'NONE',  ( 1.000000000000000000, 0.000000000000000000, 0.000000000000000000 ) ) ;
#12768 = CARTESIAN_POINT ( 'NONE',  ( 5.103531824934171013, 4.708196996972911386, -1.387778780781445676E-14 ) ) ;
#12769 = VERTEX_POINT ( 'NONE', #6955 ) ;
#12770 = VERTEX_POINT ( 'NONE', #10335 ) ;
#12771 = AXIS2_PLACEMENT_3D ( 'NONE', #6516, #6595, #3401 ) ;
#12772 = DIRECTION ( 'NONE',  ( 0.000000000000000000, 0.000000000000000000, 1.000000000000000000 ) ) ;
#12773 = DIRECTION ( 'NONE',  ( 1.000000000000000000, 0.000000000000000000, 0.000000000000000000 ) ) ;
#12774 = ORIENTED_EDGE ( 'NONE', *, *, #2464, .F. ) ;
#12775 = DIRECTION ( 'NONE',  ( 1.000000000000000000, 0.000000000000000000, 0.000000000000000000 ) ) ;
#12776 = LINE ( 'NONE', #2612, #10949 ) ;
#12777 = CARTESIAN_POINT ( 'NONE',  ( -37.00000000000000711, 29.99999999999999645, 8.000000000000007105 ) ) ;
#12778 = CARTESIAN_POINT ( 'NONE',  ( 0.000000000000000000, 25.49999999999996803, 8.000000000000007105 ) ) ;
#12779 = CONTEXT_DEPENDENT_SHAPE_REPRESENTATION ( #5497, #13185 ) ;
#12780 = DIRECTION ( 'NONE',  ( 1.892425610156517122E-16, 1.000000000000000000, 0.000000000000000000 ) ) ;
#12781 = FACE_OUTER_BOUND ( 'NONE', #2453, .T. ) ;
#12782 = DIRECTION ( 'NONE',  ( 0.000000000000000000, 0.000000000000000000, 1.000000000000000000 ) ) ;
#12783 = EDGE_CURVE ( 'NONE', #5483, #12337, #2733, .T. ) ;
#12784 = AXIS2_PLACEMENT_3D ( 'NONE', #2824, #3694, #1719 ) ;
#12785 = CARTESIAN_POINT ( 'NONE',  ( -1.642566673137935362, -4.825166380998194171, -0.07080520455422933956 ) ) ;
#12786 = APPLICATION_CONTEXT ( 'automotive_design' ) ;
#12787 = VECTOR ( 'NONE', #5298, 999.9999999999998863 ) ;
#12788 = ORIENTED_EDGE ( 'NONE', *, *, #2070, .T. ) ;
#12789 = EDGE_CURVE ( 'NONE', #3412, #14130, #7168, .T. ) ;
#12790 = ORIENTED_EDGE ( 'NONE', *, *, #13492, .T. ) ;
#12791 = CARTESIAN_POINT ( 'NONE',  ( 22.00000000000000355, 50.00000000000000000, -25.00000000000000000 ) ) ;
#12792 = EDGE_LOOP ( 'NONE', ( #7984, #5727, #7590, #12873, #12273 ) ) ;
#12793 = DIRECTION ( 'NONE',  ( 0.000000000000000000, 0.000000000000000000, 1.000000000000000000 ) ) ;
#12794 = CARTESIAN_POINT ( 'NONE',  ( -3.999999999999996447, 1.941961291383473842, -0.3515519931180204893 ) ) ;
#12795 = DIRECTION ( 'NONE',  ( -1.913084959030911013E-15, 1.000000000000000000, 0.000000000000000000 ) ) ;
#12796 = AXIS2_PLACEMENT_3D ( 'NONE', #9477, #1643, #3051 ) ;
#12797 = CARTESIAN_POINT ( 'NONE',  ( 20.00000000000000000, -5.510910596163090344E-15, 25.00000000000000000 ) ) ;
#12798 = CARTESIAN_POINT ( 'NONE',  ( 5.056385618527004411, -2.321455725013326976, -4.020879263244736990 ) ) ;
#12799 = VECTOR ( 'NONE', #654, 1000.000000000000000 ) ;
#12800 = DIRECTION ( 'NONE',  ( 0.000000000000000000, 0.000000000000000000, 1.000000000000000000 ) ) ;
#12801 = DIRECTION ( 'NONE',  ( 1.000000000000000000, 0.000000000000000000, 0.000000000000000000 ) ) ;
#12802 = CARTESIAN_POINT ( 'NONE',  ( 88.22284556172391490, -83.66032599071898801, -28.00000000000000000 ) ) ;
#12803 = DIRECTION ( 'NONE',  ( 0.000000000000000000, 0.000000000000000000, 1.000000000000000000 ) ) ;
#12804 = EDGE_CURVE ( 'NONE', #6152, #641, #1483, .T. ) ;
#12805 = PRODUCT_DEFINITION_SHAPE ( 'NONE', 'NONE',  #11881 ) ;
#12806 = DIRECTION ( 'NONE',  ( -1.000000000000000000, -1.665334536937734318E-16, 0.000000000000000000 ) ) ;
#12807 = EDGE_LOOP ( 'NONE', ( #6729, #1929, #7937, #13150 ) ) ;
#12808 = CIRCLE ( 'NONE', #7428, 2.500000000000002220 ) ;
#12809 = VECTOR ( 'NONE', #12472, 1000.000000000000000 ) ;
#12810 = CIRCLE ( 'NONE', #6484, 9.000000000000005329 ) ;
#12811 = ORIENTED_EDGE ( 'NONE', *, *, #9363, .F. ) ;
#12812 = AXIS2_PLACEMENT_3D ( 'NONE', #911, #5379, #2447 ) ;
#12813 = EDGE_CURVE ( 'NONE', #568, #3835, #4774, .T. ) ;
#12814 = EDGE_LOOP ( 'NONE', ( #10821, #8094 ) ) ;
#12815 = CARTESIAN_POINT ( 'NONE',  ( 20.00000000000000355, 50.00000000000000000, 25.00000000000000000 ) ) ;
#12816 = DIRECTION ( 'NONE',  ( 0.000000000000000000, 0.000000000000000000, 1.000000000000000000 ) ) ;
#12817 = EDGE_CURVE ( 'NONE', #10589, #12258, #8050, .T. ) ;
#12818 = AXIS2_PLACEMENT_3D ( 'NONE', #8754, #52, #7935 ) ;
#12819 = AXIS2_PLACEMENT_3D ( 'NONE', #82, #4556, #12148 ) ;
#12820 = ORIENTED_EDGE ( 'NONE', *, *, #8793, .T. ) ;
#12821 = EDGE_CURVE ( 'NONE', #7848, #6549, #3796, .T. ) ;
#12822 = AXIS2_PLACEMENT_3D ( 'NONE', #11456, #3504, #5885 ) ;
#12823 = B_SPLINE_CURVE_WITH_KNOTS ( 'NONE', 3,
 ( #1533, #6745, #1118, #12316, #7774, #3331 ),
 .UNSPECIFIED., .F., .F.,
 ( 4, 2, 4 ),
 ( 0.000000000000000000, 0.002086519881787259750, 0.004173039763574519501 ),
 .UNSPECIFIED. ) ;
#12824 = ORIENTED_EDGE ( 'NONE', *, *, #14458, .F. ) ;
#12825 = CARTESIAN_POINT ( 'NONE',  ( 118.6817075744280174, -30.42344490663937506, -117.0000000000000000 ) ) ;
#12826 = CARTESIAN_POINT ( 'NONE',  ( 0.2117491801717920341, -5.895756138069166319, -4.327903350935056181 ) ) ;
#12827 = VERTEX_POINT ( 'NONE', #12666 ) ;
#12828 =( BOUNDED_SURFACE ( )  B_SPLINE_SURFACE ( 3, 2, ( 
 ( #1778, #7166, #6067 ),
 ( #8420, #11870, #2887 ),
 ( #460, #11802, #8568 ),
 ( #6225, #5209, #8501 ),
 ( #13863, #10698, #2957 ),
 ( #7393, #1848, #10979 ) ),
 .UNSPECIFIED., .F., .F., .F. ) 
 B_SPLINE_SURFACE_WITH_KNOTS ( ( 4, 2, 4 ),
 ( 3, 3 ),
 ( 0.002450104044831693303, 0.005591829551853680358, 0.008733555058875666979 ),
 ( 0.000000000000000000, 1.000000000000000000 ),
 .UNSPECIFIED. ) 
 GEOMETRIC_REPRESENTATION_ITEM ( )  RATIONAL_B_SPLINE_SURFACE ( (
 ( 1.000000000000000000, 0.8047731410850403888, 1.000000000000000000),
 ( 1.000000000000000000, 0.8125552299157110525, 1.000000000000000000),
 ( 1.000000000000000000, 0.8191520442888694520, 1.000000000000000000),
 ( 1.000000000000000000, 0.8191520442891048193, 1.000000000000000000),
 ( 1.000000000000000000, 0.8125552299155338609, 1.000000000000000000),
 ( 1.000000000000000000, 0.8047731410850404998, 1.000000000000000000) ) ) 
 REPRESENTATION_ITEM ( '' )  SURFACE ( )  );
#12829 = PLANE ( 'NONE',  #74 ) ;
#12830 = VECTOR ( 'NONE', #1281, 1000.000000000000000 ) ;
#12831 = DIRECTION ( 'NONE',  ( -1.000000000000000000, 0.000000000000000000, 0.000000000000000000 ) ) ;
#12832 = DIRECTION ( 'NONE',  ( 0.000000000000000000, 0.000000000000000000, 1.000000000000000000 ) ) ;
#12833 = LINE ( 'NONE', #6382, #4831 ) ;
#12834 = ORIENTED_EDGE ( 'NONE', *, *, #8507, .F. ) ;
#12835 = EDGE_CURVE ( 'NONE', #11527, #11431, #4709, .T. ) ;
#12836 = CARTESIAN_POINT ( 'NONE',  ( 4.071447262713911996, 4.041451884327390331, 0.000000000000000000 ) ) ;
#12837 = CARTESIAN_POINT ( 'NONE',  ( 2.750000000000002665, 0.000000000000000000, 0.000000000000000000 ) ) ;
#12838 = VERTEX_POINT ( 'NONE', #9155 ) ;
#12839 = FACE_OUTER_BOUND ( 'NONE', #4815, .T. ) ;
#12840 = B_SPLINE_CURVE_WITH_KNOTS ( 'NONE', 3,
 ( #10781, #9686, #8574, #1712, #3112, #12993 ),
 .UNSPECIFIED., .F., .F.,
 ( 4, 2, 4 ),
 ( 0.000000000000000000, 0.001529397995383605015, 0.003058795990767210031 ),
 .UNSPECIFIED. ) ;
#12841 = LINE ( 'NONE', #7265, #11482 ) ;
#12842 = ORIENTED_EDGE ( 'NONE', *, *, #10847, .F. ) ;
#12843 = ORIENTED_EDGE ( 'NONE', *, *, #4953, .F. ) ;
#12844 = DIRECTION ( 'NONE',  ( -1.000000000000000000, -1.723842398015259277E-15, 0.000000000000000000 ) ) ;
#12845 = CARTESIAN_POINT ( 'NONE',  ( 3.540000644887140613, 2.810673041920858317, -3.302142222888913015 ) ) ;
#12846 = VECTOR ( 'NONE', #197, 1000.000000000000000 ) ;
#12847 = ORIENTED_EDGE ( 'NONE', *, *, #14119, .T. ) ;
#12848 = CARTESIAN_POINT ( 'NONE',  ( 3.200000000000000178, 5.329070518200750211E-16, 1.599999999999990319 ) ) ;
#12849 = CARTESIAN_POINT ( 'NONE',  ( 4.939003118778239276, 4.265486753573743961, 0.6119602237974551828 ) ) ;
#12850 = CIRCLE ( 'NONE', #4891, 4.000000000000000000 ) ;
#12851 = FACE_OUTER_BOUND ( 'NONE', #13562, .T. ) ;
#12852 = ORIENTED_EDGE ( 'NONE', *, *, #3622, .T. ) ;
#12853 = ORIENTED_EDGE ( 'NONE', *, *, #305, .T. ) ;
#12854 = CARTESIAN_POINT ( 'NONE',  ( 24.99999999999999289, -4.898587196589414604E-15, 25.00000000000000000 ) ) ;
#12855 = CARTESIAN_POINT ( 'NONE',  ( -0.5330603548786400081, 48.48645934998780405, 7.973110123615588130 ) ) ;
#12856 = ADVANCED_FACE ( 'NONE', ( #537 ), #3754, .T. ) ;
#12857 = ORIENTED_EDGE ( 'NONE', *, *, #14294, .F. ) ;
#12858 = VECTOR ( 'NONE', #4394, 1000.000000000000114 ) ;
#12859 = DIRECTION ( 'NONE',  ( 0.000000000000000000, 1.000000000000000000, 0.000000000000000000 ) ) ;
#12860 = DIRECTION ( 'NONE',  ( 1.000000000000000000, 0.000000000000000000, -0.000000000000000000 ) ) ;
#12861 = CARTESIAN_POINT ( 'NONE',  ( 76.68170757442801744, 29.57655509336063204, -33.00000000000000000 ) ) ;
#12862 = ORIENTED_EDGE ( 'NONE', *, *, #10171, .F. ) ;
#12863 = DIRECTION ( 'NONE',  ( 0.000000000000000000, 0.000000000000000000, -1.000000000000000000 ) ) ;
#12864 = DIRECTION ( 'NONE',  ( -1.000000000000000000, 2.312964634635741951E-14, 0.000000000000000000 ) ) ;
#12865 = CARTESIAN_POINT ( 'NONE',  ( 28.00000000000000355, 29.99999999999999645, 8.000000000000007105 ) ) ;
#12866 = CARTESIAN_POINT ( 'NONE',  ( 22.00000000000000000, 60.00000000000000711, -25.00000000000000000 ) ) ;
#12867 = CARTESIAN_POINT ( 'NONE',  ( -2.285412292771025644, -4.454019289455653841, -1.712841791506071108E-14 ) ) ;
#12868 = AXIS2_PLACEMENT_3D ( 'NONE', #3347, #7785, #4521 ) ;
#12869 = ORIENTED_EDGE ( 'NONE', *, *, #4843, .T. ) ;
#12870 = CARTESIAN_POINT ( 'NONE',  ( 0.000000000000000000, 3.031088913245536087, -1.750000000000001554 ) ) ;
#12871 = EDGE_LOOP ( 'NONE', ( #9095, #2980, #13479, #5671 ) ) ;
#12872 = EDGE_CURVE ( 'NONE', #8962, #950, #4998, .T. ) ;
#12873 = ORIENTED_EDGE ( 'NONE', *, *, #824, .F. ) ;
#12874 = CARTESIAN_POINT ( 'NONE',  ( 76.68170757442804586, 59.57655509336061073, 25.00000000000000000 ) ) ;
#12875 = EDGE_CURVE ( 'NONE', #13737, #9480, #1397, .T. ) ;
#12876 = DIRECTION ( 'NONE',  ( 1.000000000000000000, 0.000000000000000000, 0.000000000000000000 ) ) ;
#12877 = CARTESIAN_POINT ( 'NONE',  ( -108.6817075744279890, 189.5765550933605823, -106.9999999999999858 ) ) ;
#12878 = CIRCLE ( 'NONE', #10989, 2.375000000000000000 ) ;
#12879 = CARTESIAN_POINT ( 'NONE',  ( 5.000882498481302285, -2.309401076758511806, -3.999999999999989786 ) ) ;
#12880 = MECHANICAL_DESIGN_GEOMETRIC_PRESENTATION_REPRESENTATION (  '', ( #13344 ), #3071 ) ;
#12881 = ORIENTED_EDGE ( 'NONE', *, *, #6925, .F. ) ;
#12882 = FACE_OUTER_BOUND ( 'NONE', #4509, .T. ) ;
#12883 = SHAPE_DEFINITION_REPRESENTATION ( #10458, #4432 ) ;
#12884 = CARTESIAN_POINT ( 'NONE',  ( 2.449848172108562760, 3.432307619358744066, -3.203702292528890272 ) ) ;
#12885 = APPLICATION_CONTEXT ( 'automotive_design' ) ;
#12886 = CIRCLE ( 'NONE', #12632, 2.600000000000004974 ) ;
#12887 = CARTESIAN_POINT ( 'NONE',  ( 25.39999999999999858, 29.99999999999999645, -24.99999999999999289 ) ) ;
#12888 = ADVANCED_FACE ( 'NONE', ( #7026 ), #1549, .F. ) ;
#12889 = DIRECTION ( 'NONE',  ( 0.000000000000000000, 1.000000000000000000, 0.000000000000000000 ) ) ;
#12890 = CIRCLE ( 'NONE', #7731, 2.100000000000000977 ) ;
#12891 = ORIENTED_EDGE ( 'NONE', *, *, #4108, .F. ) ;
#12892 = AXIS2_PLACEMENT_3D ( 'NONE', #8678, #8817, #7859 ) ;
#12893 = ORIENTED_EDGE ( 'NONE', *, *, #13005, .F. ) ;
#12894 = AXIS2_PLACEMENT_3D ( 'NONE', #4772, #9222, #11285 ) ;
#12895 = ADVANCED_FACE ( 'NONE', ( #11497 ), #14331, .F. ) ;
#12896 = EDGE_CURVE ( 'NONE', #11268, #73, #1996, .T. ) ;
#12897 = DIRECTION ( 'NONE',  ( -0.2425356250363327748, 0.9701425001453319874, 0.000000000000000000 ) ) ;
#12898 = CARTESIAN_POINT ( 'NONE',  ( -28.00000000000000355, 35.49999999999997868, 0.000000000000000000 ) ) ;
#12899 = EDGE_CURVE ( 'NONE', #10272, #1545, #8343, .T. ) ;
#12900 = VECTOR ( 'NONE', #14412, 1000.000000000000000 ) ;
#12901 = ORIENTED_EDGE ( 'NONE', *, *, #2982, .T. ) ;
#12902 = PRESENTATION_LAYER_ASSIGNMENT (  '', '', ( #4269 ) ) ;
#12903 = VECTOR ( 'NONE', #2640, 1000.000000000000000 ) ;
#12904 = LINE ( 'NONE', #11570, #10462 ) ;
#12905 = CARTESIAN_POINT ( 'NONE',  ( -3.417629563435960804, -3.800333343456104185, -4.019399823475084510 ) ) ;
#12906 = EDGE_LOOP ( 'NONE', ( #11132, #2138, #5293, #11141, #11424, #10779, #12322, #13057, #7434 ) ) ;
#12907 = EDGE_CURVE ( 'NONE', #5824, #14008, #6434, .T. ) ;
#12908 = LINE ( 'NONE', #13135, #9667 ) ;
#12909 = EDGE_LOOP ( 'NONE', ( #12489, #4845, #11994, #10397, #3746, #7046, #14428, #1768, #13655, #11864, #10722, #10002 ) ) ;
#12910 = VECTOR ( 'NONE', #2019, 1000.000000000000000 ) ;
#12911 = EDGE_LOOP ( 'NONE', ( #12363, #7560, #12893, #11569 ) ) ;
#12912 = AXIS2_PLACEMENT_3D ( 'NONE', #6299, #13054, #1849 ) ;
#12913 = AXIS2_PLACEMENT_3D ( 'NONE', #7447, #1832, #14138 ) ;
#12914 = EDGE_CURVE ( 'NONE', #2673, #7600, #8913, .T. ) ;
#12915 = DIRECTION ( 'NONE',  ( -1.000000000000000000, -3.286707217423839940E-17, -2.273843122241288053E-18 ) ) ;
#12916 = CYLINDRICAL_SURFACE ( 'NONE', #10410, 2.750000000000003997 ) ;
#12917 = FACE_OUTER_BOUND ( 'NONE', #2807, .T. ) ;
#12918 = EDGE_CURVE ( 'NONE', #1783, #9506, #11949, .T. ) ;
#12919 = ORIENTED_EDGE ( 'NONE', *, *, #1999, .F. ) ;
#12920 = CARTESIAN_POINT ( 'NONE',  ( -5.248984340851197139, -2.531668808681911909, -4.566868479993924090 ) ) ;
#12921 = CARTESIAN_POINT ( 'NONE',  ( 4.938994369585081756, -1.602723107909851619, -4.000000000000001776 ) ) ;
#12922 = ORIENTED_EDGE ( 'NONE', *, *, #2745, .T. ) ;
#12923 = CARTESIAN_POINT ( 'NONE',  ( 4.966167347451064806, 4.334074124826262420, -0.6428484488893171367 ) ) ;
#12924 = DIRECTION ( 'NONE',  ( 1.723842398015259277E-15, -1.000000000000000000, 0.000000000000000000 ) ) ;
#12925 = EDGE_LOOP ( 'NONE', ( #12225, #6172, #11355, #4142, #2159, #8432, #8092 ) ) ;
#12926 = B_SPLINE_CURVE_WITH_KNOTS ( 'NONE', 3,
 ( #10354, #3701, #8141, #4151, #10792 ),
 .UNSPECIFIED., .F., .F.,
 ( 4, 1, 4 ),
 ( 0.000000000000000000, 0.002309401076758505356, 0.004618802153517010713 ),
 .UNSPECIFIED. ) ;
#12927 = DIRECTION ( 'NONE',  ( -1.000000000000000000, 0.000000000000000000, 0.000000000000000000 ) ) ;
#12928 = VERTEX_POINT ( 'NONE', #9602 ) ;
#12929 = DIRECTION ( 'NONE',  ( 1.000000000000000000, 1.665334536937734071E-16, 0.000000000000000000 ) ) ;
#12930 = STYLED_ITEM ( 'NONE', ( #2074 ), #8181 ) ;
#12931 = VECTOR ( 'NONE', #8041, 1000.000000000000000 ) ;
#12932 = CIRCLE ( 'NONE', #77, 3.000000000000001332 ) ;
#12933 = CARTESIAN_POINT ( 'NONE',  ( 22.00000000000000355, 27.00000000000000355, -25.00000000000000000 ) ) ;
#12934 = ORIENTED_EDGE ( 'NONE', *, *, #4029, .F. ) ;
#12935 = CARTESIAN_POINT ( 'NONE',  ( 20.00000000000000000, -5.510910596163090344E-15, -25.00000000000000000 ) ) ;
#12936 = EDGE_CURVE ( 'NONE', #8895, #13013, #3366, .T. ) ;
#12937 = EDGE_CURVE ( 'NONE', #4466, #1176, #5282, .T. ) ;
#12938 = CARTESIAN_POINT ( 'NONE',  ( 51.90514726928103073, 42.68717498692012668, 25.00000000000000000 ) ) ;
#12939 = DIRECTION ( 'NONE',  ( 1.000000000000000000, 1.665334536937734071E-16, 0.000000000000000000 ) ) ;
#12940 = ORIENTED_EDGE ( 'NONE', *, *, #12720, .T. ) ;
#12941 = ORIENTED_EDGE ( 'NONE', *, *, #9630, .T. ) ;
#12942 = FACE_OUTER_BOUND ( 'NONE', #1874, .T. ) ;
#12943 = DIRECTION ( 'NONE',  ( 0.000000000000000000, 0.000000000000000000, 1.000000000000000000 ) ) ;
#12944 = ORIENTED_EDGE ( 'NONE', *, *, #1445, .F. ) ;
#12945 = CARTESIAN_POINT ( 'NONE',  ( 5.067058822021064834, -2.325541950156881033, 4.027956812804549536 ) ) ;
#12946 = VECTOR ( 'NONE', #7171, 999.9999999999998863 ) ;
#12947 = PRODUCT_DEFINITION_SHAPE ( 'NONE', 'NONE',  #14482 ) ;
#12948 = CARTESIAN_POINT ( 'NONE',  ( 47.05443476855437268, 62.09002498982675888, 25.00000000000000000 ) ) ;
#12949 = PLANE ( 'NONE',  #2545 ) ;
#12950 = DIRECTION ( 'NONE',  ( 0.000000000000000000, 0.000000000000000000, -1.000000000000000000 ) ) ;
#12951 = EDGE_LOOP ( 'NONE', ( #3880, #4800, #3861, #4791 ) ) ;
#12952 = DIRECTION ( 'NONE',  ( -1.000000000000000000, 2.551526159633733968E-19, 1.987661601597216239E-18 ) ) ;
#12953 = DIRECTION ( 'NONE',  ( 0.000000000000000000, 0.000000000000000000, 1.000000000000000000 ) ) ;
#12954 = DIRECTION ( 'NONE',  ( -2.273843122241288438E-18, -5.551115123125783935E-17, -1.000000000000000000 ) ) ;
#12955 = ADVANCED_FACE ( 'NONE', ( #14083 ), #14010, .T. ) ;
#12956 = CONICAL_SURFACE ( 'NONE', #315, 2.500000000000002220, 0.9599310885968781459 ) ;
#12957 = EDGE_LOOP ( 'NONE', ( #8073, #5225, #9099 ) ) ;
#12958 = ORIENTED_EDGE ( 'NONE', *, *, #3769, .T. ) ;
#12959 = B_SPLINE_CURVE_WITH_KNOTS ( 'NONE', 3,
 ( #7364, #14048, #13962, #5094 ),
 .UNSPECIFIED., .F., .F.,
 ( 4, 4 ),
 ( 0.002080789711329273685, 0.004173039763574509092 ),
 .UNSPECIFIED. ) ;
#12960 = VECTOR ( 'NONE', #6046, 1000.000000000000000 ) ;
#12961 = DIRECTION ( 'NONE',  ( 0.000000000000000000, 0.000000000000000000, 1.000000000000000000 ) ) ;
#12962 = EDGE_LOOP ( 'NONE', ( #11231, #11296 ) ) ;
#12963 = ORIENTED_EDGE ( 'NONE', *, *, #7052, .F. ) ;
#12964 = EDGE_CURVE ( 'NONE', #13190, #4994, #7291, .T. ) ;
#12965 = DIRECTION ( 'NONE',  ( -1.000000000000000000, 0.000000000000000000, 0.000000000000000000 ) ) ;
#12966 = DIRECTION ( 'NONE',  ( 0.000000000000000000, 0.000000000000000000, 1.000000000000000000 ) ) ;
#12967 = AXIS2_PLACEMENT_3D ( 'NONE', #9063, #3524, #7965 ) ;
#12968 = LINE ( 'NONE', #14134, #3053 ) ;
#12969 = DIRECTION ( 'NONE',  ( 3.286707217423839940E-17, -1.000000000000000000, 5.551115123125782702E-17 ) ) ;
#12970 = CARTESIAN_POINT ( 'NONE',  ( 62.10586122665989706, -20.42344490663939993, -28.00000000000000000 ) ) ;
#12971 = CONTEXT_DEPENDENT_SHAPE_REPRESENTATION ( #7539, #4626 ) ;
#12972 = CARTESIAN_POINT ( 'NONE',  ( 0.6920835326022568568, 4.454600218803893341, -3.297382984111599580 ) ) ;
#12973 = DIRECTION ( 'NONE',  ( 0.000000000000000000, 0.000000000000000000, 1.000000000000000000 ) ) ;
#12974 = AXIS2_PLACEMENT_3D ( 'NONE', #3132, #2018, #5374 ) ;
#12975 = ORIENTED_EDGE ( 'NONE', *, *, #4352, .F. ) ;
#12976 = EDGE_CURVE ( 'NONE', #269, #10405, #5647, .T. ) ;
#12977 = EDGE_CURVE ( 'NONE', #2995, #10278, #7394, .T. ) ;
#12978 = CARTESIAN_POINT ( 'NONE',  ( 1.738710530748207583, 5.045296470309983405, -4.385927688751852571 ) ) ;
#12979 = ORIENTED_EDGE ( 'NONE', *, *, #522, .T. ) ;
#12980 = DIRECTION ( 'NONE',  ( -1.000000000000000000, 0.000000000000000000, 0.000000000000000000 ) ) ;
#12981 = ORIENTED_EDGE ( 'NONE', *, *, #3243, .T. ) ;
#12982 = ORIENTED_EDGE ( 'NONE', *, *, #11110, .F. ) ;
#12983 = DIRECTION ( 'NONE',  ( 0.000000000000000000, 0.000000000000000000, 1.000000000000000000 ) ) ;
#12984 = CARTESIAN_POINT ( 'NONE',  ( 33.99999999999998579, 80.00000000000000000, -25.00000000000000000 ) ) ;
#12985 = SURFACE_SIDE_STYLE ('',( #2134 ) ) ;
#12986 = ORIENTED_EDGE ( 'NONE', *, *, #11110, .T. ) ;
#12987 = PLANE ( 'NONE',  #13517 ) ;
#12988 = CARTESIAN_POINT ( 'NONE',  ( 79.68170757442804586, 124.5765550933606249, 25.00000000000000000 ) ) ;
#12989 = ORIENTED_EDGE ( 'NONE', *, *, #10400, .F. ) ;
#12990 = PLANE ( 'NONE',  #9895 ) ;
#12991 = VERTEX_POINT ( 'NONE', #1926 ) ;
#12992 = DIRECTION ( 'NONE',  ( 0.000000000000000000, 0.000000000000000000, -1.000000000000000000 ) ) ;
#12993 = CARTESIAN_POINT ( 'NONE',  ( 5.236872748402767286, 8.765285303662936917E-14, -4.357689166958464533 ) ) ;
#12994 = DIRECTION ( 'NONE',  ( 1.000000000000000000, 1.665334536937734071E-16, 0.000000000000000000 ) ) ;
#12995 = ORIENTED_EDGE ( 'NONE', *, *, #12720, .F. ) ;
#12996 = LINE ( 'NONE', #627, #14054 ) ;
#12997 = CARTESIAN_POINT ( 'NONE',  ( 4.870929040049785108, -0.7939434348317983003, -4.072348019690683607 ) ) ;
#12998 = ORIENTED_EDGE ( 'NONE', *, *, #10911, .F. ) ;
#12999 = AXIS2_PLACEMENT_3D ( 'NONE', #5654, #10131, #116 ) ;
#13000 = CARTESIAN_POINT ( 'NONE',  ( 30.00229726637438432, 120.2985749985466839, 25.00000000000000000 ) ) ;
#13001 = EDGE_LOOP ( 'NONE', ( #2050, #11042 ) ) ;
#13002 = VERTEX_POINT ( 'NONE', #9742 ) ;
#13003 = DIRECTION ( 'NONE',  ( 0.9701425001453319874, 0.2425356250363330801, 0.000000000000000000 ) ) ;
#13004 = CARTESIAN_POINT ( 'NONE',  ( -0.1404055950190682134, -4.699865361597010960, -3.386887224136959862 ) ) ;
#13005 = EDGE_CURVE ( 'NONE', #6697, #7073, #4921, .T. ) ;
#13006 = ORIENTED_EDGE ( 'NONE', *, *, #13970, .F. ) ;
#13007 = DIRECTION ( 'NONE',  ( 0.000000000000000000, -8.482162385747133845E-47, 1.000000000000000000 ) ) ;
#13008 = EDGE_CURVE ( 'NONE', #1563, #13498, #97, .T. ) ;
#13009 = CARTESIAN_POINT ( 'NONE',  ( 0.000000000000000000, 0.000000000000000000, -25.03750572909319061 ) ) ;
#13010 = B_SPLINE_CURVE_WITH_KNOTS ( 'NONE', 3,
 ( #11333, #3663, #11551, #364, #11401, #9282 ),
 .UNSPECIFIED., .F., .F.,
 ( 4, 2, 4 ),
 ( 0.000000000000000000, 0.0002514304509865741182, 0.0005028609019731482364 ),
 .UNSPECIFIED. ) ;
#13011 = VECTOR ( 'NONE', #11736, 999.9999999999998863 ) ;
#13012 = VERTEX_POINT ( 'NONE', #14367 ) ;
#13013 = VERTEX_POINT ( 'NONE', #12308 ) ;
#13014 = LINE ( 'NONE', #12045, #7091 ) ;
#13015 = CARTESIAN_POINT ( 'NONE',  ( -3.588625829919864341, 47.65084415347212854, 5.785846103500081661 ) ) ;
#13016 = ORIENTED_EDGE ( 'NONE', *, *, #1174, .T. ) ;
#13017 = DIRECTION ( 'NONE',  ( 0.000000000000000000, -0.4999999999999997224, 0.8660254037844387076 ) ) ;
#13018 = DIRECTION ( 'NONE',  ( 1.000000000000000000, 0.000000000000000000, 0.000000000000000000 ) ) ;
#13019 = EDGE_CURVE ( 'NONE', #8446, #7155, #11747, .T. ) ;
#13020 = CARTESIAN_POINT ( 'NONE',  ( 4.030875481282749639, 1.403567514398344596, 3.499999999999992006 ) ) ;
#13021 = DIRECTION ( 'NONE',  ( 1.000000000000000000, 0.000000000000000000, 0.000000000000000000 ) ) ;
#13022 = LINE ( 'NONE', #1886, #426 ) ;
#13023 = EDGE_CURVE ( 'NONE', #12697, #11527, #12239, .T. ) ;
#13024 = CARTESIAN_POINT ( 'NONE',  ( 4.191707736911188142, -3.353419101626373244, -0.2701150775514071789 ) ) ;
#13025 = ORIENTED_EDGE ( 'NONE', *, *, #11822, .T. ) ;
#13026 = VERTEX_POINT ( 'NONE', #13342 ) ;
#13027 = FACE_OUTER_BOUND ( 'NONE', #2440, .T. ) ;
#13028 = ORIENTED_EDGE ( 'NONE', *, *, #1593, .F. ) ;
#13029 = ORIENTED_EDGE ( 'NONE', *, *, #8491, .F. ) ;
#13030 = CARTESIAN_POINT ( 'NONE',  ( -118.6817075744282306, 109.5765550933602697, 0.000000000000000000 ) ) ;
#13031 = LINE ( 'NONE', #1974, #2100 ) ;
#13032 = CARTESIAN_POINT ( 'NONE',  ( 3.588625829919864785, 47.65084415347212143, 5.785846103500077220 ) ) ;
#13033 = EDGE_CURVE ( 'NONE', #11584, #8618, #3242, .T. ) ;
#13034 = CARTESIAN_POINT ( 'NONE',  ( 22.00000000000000000, 67.00000000000000000, -25.00000000000000000 ) ) ;
#13035 = VECTOR ( 'NONE', #2738, 1000.000000000000000 ) ;
#13036 = DIRECTION ( 'NONE',  ( -1.000000000000000000, 0.000000000000000000, -0.000000000000000000 ) ) ;
#13037 = SHAPE_DEFINITION_REPRESENTATION ( #1467, #3865 ) ;
#13038 = FACE_BOUND ( 'NONE', #3296, .T. ) ;
#13039 = DIRECTION ( 'NONE',  ( -1.000000000000000000, 0.000000000000000000, 0.000000000000000000 ) ) ;
#13040 = EDGE_LOOP ( 'NONE', ( #1479, #14141, #10173, #12986 ) ) ;
#13041 = DIRECTION ( 'NONE',  ( 0.000000000000000000, 0.000000000000000000, 1.000000000000000000 ) ) ;
#13042 = EDGE_LOOP ( 'NONE', ( #10793, #9986, #13619, #13322 ) ) ;
#13043 = VERTEX_POINT ( 'NONE', #9892 ) ;
#13044 = VECTOR ( 'NONE', #6094, 1000.000000000000000 ) ;
#13045 = VECTOR ( 'NONE', #10564, 1000.000000000000000 ) ;
#13046 = DIRECTION ( 'NONE',  ( 0.000000000000000000, 0.000000000000000000, -1.000000000000000000 ) ) ;
#13047 = DIRECTION ( 'NONE',  ( 0.000000000000000000, 0.000000000000000000, -1.000000000000000000 ) ) ;
#13048 = EDGE_CURVE ( 'NONE', #2724, #3412, #5423, .T. ) ;
#13049 = EDGE_CURVE ( 'NONE', #8895, #7559, #11985, .T. ) ;
#13050 = ORIENTED_EDGE ( 'NONE', *, *, #5928, .F. ) ;
#13051 = CIRCLE ( 'NONE', #4657, 4.000000000000000888 ) ;
#13052 = CARTESIAN_POINT ( 'NONE',  ( -140.0000000000003411, 189.5765550933606107, 47.99999999999998579 ) ) ;
#13053 = AXIS2_PLACEMENT_3D ( 'NONE', #1080, #5536, #9791 ) ;
#13054 = DIRECTION ( 'NONE',  ( -0.000000000000000000, -0.000000000000000000, -1.000000000000000000 ) ) ;
#13055 = CARTESIAN_POINT ( 'NONE',  ( 20.00000000000000355, 50.00000000000000000, 25.00000000000000000 ) ) ;
#13056 = ORIENTED_EDGE ( 'NONE', *, *, #283, .F. ) ;
#13057 = ORIENTED_EDGE ( 'NONE', *, *, #9805, .F. ) ;
#13058 = UNCERTAINTY_MEASURE_WITH_UNIT (LENGTH_MEASURE( 1.000000000000000082E-05 ), #10642, 'distance_accuracy_value', 'NONE');
#13059 = DIRECTION ( 'NONE',  ( 0.000000000000000000, 0.000000000000000000, -1.000000000000000000 ) ) ;
#13060 = DIRECTION ( 'NONE',  ( 0.000000000000000000, 0.000000000000000000, -1.000000000000000000 ) ) ;
#13061 = PLANE ( 'NONE',  #9268 ) ;
#13062 = VECTOR ( 'NONE', #5281, 1000.000000000000000 ) ;
#13063 = EDGE_LOOP ( 'NONE', ( #13521, #8271, #7842, #8026 ) ) ;
#13064 = EDGE_CURVE ( 'NONE', #13624, #6890, #9813, .T. ) ;
#13065 = VECTOR ( 'NONE', #1137, 1000.000000000000227 ) ;
#13066 = CARTESIAN_POINT ( 'NONE',  ( 4.082498951862935321, 4.041451884327390331, 2.512980736064700723E-20 ) ) ;
#13067 = CARTESIAN_POINT ( 'NONE',  ( 4.962655643710850661, -1.591468071165726528, -4.074777072973637893 ) ) ;
#13068 = EDGE_CURVE ( 'NONE', #11163, #11314, #4738, .T. ) ;
#13069 = SURFACE_STYLE_USAGE ( .BOTH. , #7693 ) ;
#13070 = DIRECTION ( 'NONE',  ( 0.000000000000000000, 0.000000000000000000, -1.000000000000000000 ) ) ;
#13071 = VERTEX_POINT ( 'NONE', #8787 ) ;
#13072 = ORIENTED_EDGE ( 'NONE', *, *, #3622, .F. ) ;
#13073 = DIRECTION ( 'NONE',  ( -1.000000000000000000, 0.000000000000000000, -0.000000000000000000 ) ) ;
#13074 = DIRECTION ( 'NONE',  ( -0.000000000000000000, -0.000000000000000000, -1.000000000000000000 ) ) ;
#13075 = VERTEX_POINT ( 'NONE', #10980 ) ;
#13076 = CARTESIAN_POINT ( 'NONE',  ( 1.560000000000005826, 1.732050807568871864, 0.000000000000000000 ) ) ;
#13077 = CARTESIAN_POINT ( 'NONE',  ( 5.029396762153807821, -2.903723574490948423, -4.451008977024202729 ) ) ;
#13078 = VECTOR ( 'NONE', #3447, 1000.000000000000114 ) ;
#13079 = VERTEX_POINT ( 'NONE', #5496 ) ;
#13080 = ORIENTED_EDGE ( 'NONE', *, *, #8136, .T. ) ;
#13081 = FACE_OUTER_BOUND ( 'NONE', #4517, .T. ) ;
#13082 = LINE ( 'NONE', #3133, #6816 ) ;
#13083 = ORIENTED_EDGE ( 'NONE', *, *, #13856, .F. ) ;
#13084 = CARTESIAN_POINT ( 'NONE',  ( 4.093692494532779946, -4.043567292011558401, 1.064034557724744967E-16 ) ) ;
#13085 = LINE ( 'NONE', #593, #10299 ) ;
#13086 = EDGE_CURVE ( 'NONE', #12252, #10954, #11061, .T. ) ;
#13087 = EDGE_CURVE ( 'NONE', #9008, #8394, #5634, .T. ) ;
#13088 = DIRECTION ( 'NONE',  ( -0.000000000000000000, -0.000000000000000000, -1.000000000000000000 ) ) ;
#13089 = CARTESIAN_POINT ( 'NONE',  ( 0.000000000000000000, 40.49999999999999289, 8.000000000000007105 ) ) ;
#13090 = PLANE ( 'NONE',  #12615 ) ;
#13091 = EDGE_CURVE ( 'NONE', #9797, #11904, #3322, .T. ) ;
#13092 = CARTESIAN_POINT ( 'NONE',  ( 5.253368672218637236, -3.033033817057797510, -4.659491423763650886 ) ) ;
#13093 = DIRECTION ( 'NONE',  ( 1.000000000000000000, 3.286707217423839940E-17, 2.273843122241288053E-18 ) ) ;
#13094 = EDGE_CURVE ( 'NONE', #777, #4680, #4284, .T. ) ;
#13095 = ADVANCED_FACE ( 'NONE', ( #9964 ), #10031, .F. ) ;
#13096 = EDGE_LOOP ( 'NONE', ( #3161, #5123 ) ) ;
#13097 = ORIENTED_EDGE ( 'NONE', *, *, #6631, .F. ) ;
#13098 = CIRCLE ( 'NONE', #7920, 2.540000000000002700 ) ;
#13099 = CARTESIAN_POINT ( 'NONE',  ( 6.800000000000028244, -6.938893903907228378E-15, 0.000000000000000000 ) ) ;
#13100 = ORIENTED_EDGE ( 'NONE', *, *, #11143, .F. ) ;
#13101 = ORIENTED_EDGE ( 'NONE', *, *, #4693, .F. ) ;
#13102 = FACE_OUTER_BOUND ( 'NONE', #4640, .T. ) ;
#13103 = AXIS2_PLACEMENT_3D ( 'NONE', #9954, #3308, #8846 ) ;
#13104 = EDGE_CURVE ( 'NONE', #8097, #6195, #3174, .T. ) ;
#13105 = CARTESIAN_POINT ( 'NONE',  ( 5.238715782502664453, -1.018209582082216347, -4.386015505371676504 ) ) ;
#13106 = CARTESIAN_POINT ( 'NONE',  ( 62.10586122665984732, -20.42344490663941414, 35.00000000000000000 ) ) ;
#13107 = DIRECTION ( 'NONE',  ( -1.000000000000000000, 0.000000000000000000, -0.000000000000000000 ) ) ;
#13108 = CARTESIAN_POINT ( 'NONE',  ( 31.44014396567294867, 38.31657438465161647, 8.000000000000007105 ) ) ;
#13109 = APPLICATION_PROTOCOL_DEFINITION ( 'draft international standard', 'automotive_design', 1998, #12885 ) ;
#13110 = CARTESIAN_POINT ( 'NONE',  ( 4.000000000001417533, -1.677829075513190160, -3.235264651232573119 ) ) ;
#13111 = CARTESIAN_POINT ( 'NONE',  ( 20.00000000000000000, -5.510910596163090344E-15, -25.00000000000000000 ) ) ;
#13112 = ADVANCED_BREP_SHAPE_REPRESENTATION ( '', ( #1904, #11025 ), #1463 ) ;
#13113 = VECTOR ( 'NONE', #5818, 1000.000000000000000 ) ;
#13114 = ADVANCED_FACE ( 'NONE', ( #10105 ), #6660, .T. ) ;
#13115 = EDGE_LOOP ( 'NONE', ( #4655, #9152, #4985, #8220 ) ) ;
#13116 = DIRECTION ( 'NONE',  ( -1.000000000000000000, 0.000000000000000000, 0.000000000000000000 ) ) ;
#13117 = ORIENTED_EDGE ( 'NONE', *, *, #9460, .T. ) ;
#13118 = ADVANCED_FACE ( 'NONE', ( #6734, #7906 ), #955, .F. ) ;
#13119 = DIRECTION ( 'NONE',  ( 0.000000000000000000, 0.000000000000000000, 1.000000000000000000 ) ) ;
#13120 = ORIENTED_EDGE ( 'NONE', *, *, #8557, .T. ) ;
#13121 = AXIS2_PLACEMENT_3D ( 'NONE', #1441, #351, #13748 ) ;
#13122 = VECTOR ( 'NONE', #1132, 1000.000000000000000 ) ;
#13123 = PLANE ( 'NONE',  #8935 ) ;
#13124 = CARTESIAN_POINT ( 'NONE',  ( 8.000000000000000000, 40.49999999999999289, 8.000000000000007105 ) ) ;
#13125 = AXIS2_PLACEMENT_3D ( 'NONE', #6022, #566, #6185 ) ;
#13126 = DIRECTION ( 'NONE',  ( 1.000000000000000000, 0.000000000000000000, 0.000000000000000000 ) ) ;
#13127 = EDGE_CURVE ( 'NONE', #435, #13438, #4351, .T. ) ;
#13128 = ORIENTED_EDGE ( 'NONE', *, *, #868, .T. ) ;
#13129 = ORIENTED_EDGE ( 'NONE', *, *, #11068, .T. ) ;
#13130 = CYLINDRICAL_SURFACE ( 'NONE', #2773, 2.500000000000002220 ) ;
#13131 = VECTOR ( 'NONE', #6652, 1000.000000000000000 ) ;
#13132 = VECTOR ( 'NONE', #12407, 1000.000000000000000 ) ;
#13133 = CARTESIAN_POINT ( 'NONE',  ( 3.332577314687724973E-15, 5.773502691896274186, -4.369520038198757561 ) ) ;
#13134 = EDGE_CURVE ( 'NONE', #13727, #14013, #12512, .T. ) ;
#13135 = CARTESIAN_POINT ( 'NONE',  ( 22.00000000000000711, 20.00000000000000355, -25.00000000000000000 ) ) ;
#13136 = AXIS2_PLACEMENT_3D ( 'NONE', #3465, #1260, #7093 ) ;
#13137 = DIRECTION ( 'NONE',  ( -0.000000000000000000, -1.000000000000000000, 0.000000000000000000 ) ) ;
#13138 = CARTESIAN_POINT ( 'NONE',  ( -2.976897293125237753E-15, -3.202582148906733206, -1.452965002680418616 ) ) ;
#13139 = DIRECTION ( 'NONE',  ( -0.000000000000000000, -1.000000000000000000, -0.000000000000000000 ) ) ;
#13140 = VECTOR ( 'NONE', #9584, 1000.000000000000000 ) ;
#13141 = FACE_OUTER_BOUND ( 'NONE', #11844, .T. ) ;
#13142 =( GEOMETRIC_REPRESENTATION_CONTEXT ( 3 ) GLOBAL_UNCERTAINTY_ASSIGNED_CONTEXT ( ( #14088 ) ) GLOBAL_UNIT_ASSIGNED_CONTEXT ( ( #12155, #6504, #14149 ) ) REPRESENTATION_CONTEXT ( 'NONE', 'WORKASPACE' ) );
#13143 = CIRCLE ( 'NONE', #7497, 2.499999999999999556 ) ;
#13144 = CARTESIAN_POINT ( 'NONE',  ( 0.6666666666666671848, 4.233901974057268092, -3.000726591567076440 ) ) ;
#13145 = FILL_AREA_STYLE ('',( #14378 ) ) ;
#13146 = CARTESIAN_POINT ( 'NONE',  ( 68.68170757442801744, 39.57655509336063915, -106.9999999999999858 ) ) ;
#13147 = ORIENTED_EDGE ( 'NONE', *, *, #11457, .F. ) ;
#13148 = FACE_OUTER_BOUND ( 'NONE', #4581, .T. ) ;
#13149 = LINE ( 'NONE', #776, #7289 ) ;
#13150 = ORIENTED_EDGE ( 'NONE', *, *, #8957, .F. ) ;
#13151 = DIRECTION ( 'NONE',  ( 0.000000000000000000, 5.551115123125782702E-17, 1.000000000000000000 ) ) ;
#13152 = EDGE_CURVE ( 'NONE', #11358, #7747, #1470, .T. ) ;
#13153 = DIRECTION ( 'NONE',  ( 1.000000000000000000, 3.286707217423839940E-17, 2.273843122241288053E-18 ) ) ;
#13154 = AXIS2_PLACEMENT_3D ( 'NONE', #10789, #10856, #769 ) ;
#13155 = EDGE_CURVE ( 'NONE', #2725, #8584, #4694, .T. ) ;
#13156 = ORIENTED_EDGE ( 'NONE', *, *, #2411, .F. ) ;
#13157 = EDGE_LOOP ( 'NONE', ( #1627, #4463, #4157 ) ) ;
#13158 = CARTESIAN_POINT ( 'NONE',  ( -2.069940739436577193, 4.578421848775986014, -3.163668057994810583E-15 ) ) ;
#13159 = CARTESIAN_POINT ( 'NONE',  ( -3.999740995676851707, 47.42835276639851116, 4.270072082080264231 ) ) ;
#13160 = ORIENTED_EDGE ( 'NONE', *, *, #999, .T. ) ;
#13161 = CARTESIAN_POINT ( 'NONE',  ( 5.098157279264019515, -2.347014727359296948, 4.065148753898753853 ) ) ;
#13162 = CARTESIAN_POINT ( 'NONE',  ( 0.000000000000000000, 0.000000000000000000, 1.599999999999990319 ) ) ;
#13163 = CARTESIAN_POINT ( 'NONE',  ( 18.68170757442808849, 141.2731697022877313, -23.00000000000000000 ) ) ;
#13164 = DIRECTION ( 'NONE',  ( 1.000000000000000000, 0.000000000000000000, 0.000000000000000000 ) ) ;
#13165 = AXIS2_PLACEMENT_3D ( 'NONE', #304, #3824, #11561 ) ;
#13166 = CARTESIAN_POINT ( 'NONE',  ( -4.000000000000000000, -2.309401076758511806, -4.699999999999981526 ) ) ;
#13167 = B_SPLINE_CURVE_WITH_KNOTS ( 'NONE', 3,
 ( #2610, #10211, #8012, #6983, #11454, #1514 ),
 .UNSPECIFIED., .F., .F.,
 ( 4, 2, 4 ),
 ( 0.01103795673506155484, 0.01206113197427181871, 0.01308430721348208085 ),
 .UNSPECIFIED. ) ;
#13168 = CARTESIAN_POINT ( 'NONE',  ( 4.871660775260050258, 3.136983646853265029, -2.711317785102856259 ) ) ;
#13169 = B_SPLINE_CURVE_WITH_KNOTS ( 'NONE', 3,
 ( #1866, #10791, #6090, #559, #5015, #13946, #3997, #772 ),
 .UNSPECIFIED., .F., .F.,
 ( 4, 2, 2, 4 ),
 ( 2.451332856815838846E-07, 0.001475502392055680735, 0.002213131021440680520, 0.002950759650825679654 ),
 .UNSPECIFIED. ) ;
#13170 = FACE_OUTER_BOUND ( 'NONE', #12044, .T. ) ;
#13171 = VERTEX_POINT ( 'NONE', #9292 ) ;
#13172 = VERTEX_POINT ( 'NONE', #1536 ) ;
#13173 = CIRCLE ( 'NONE', #2641, 5.384454397937120440 ) ;
#13174 = EDGE_LOOP ( 'NONE', ( #13451, #7963, #6713, #1508 ) ) ;
#13175 = LINE ( 'NONE', #5391, #1252 ) ;
#13176 = ORIENTED_EDGE ( 'NONE', *, *, #7433, .F. ) ;
#13177 = CARTESIAN_POINT ( 'NONE',  ( 28.00000000000000355, 29.99999999999999645, 6.999999999999992006 ) ) ;
#13178 = CARTESIAN_POINT ( 'NONE',  ( -2.500000000000011990, 4.330127018922186544, 0.000000000000000000 ) ) ;
#13179 = DIRECTION ( 'NONE',  ( 0.000000000000000000, 5.551115123125782702E-17, 1.000000000000000000 ) ) ;
#13180 = CARTESIAN_POINT ( 'NONE',  ( -37.00000000000000711, 29.99999999999999645, 0.000000000000000000 ) ) ;
#13181 = DIRECTION ( 'NONE',  ( -1.000000000000000000, -3.286707217423839940E-17, -2.273843122241288053E-18 ) ) ;
#13182 = SHAPE_DEFINITION_REPRESENTATION ( #171, #8802 ) ;
#13183 = CARTESIAN_POINT ( 'NONE',  ( 4.204114824917655646, -1.660420935435633627, -3.302147294767053154 ) ) ;
#13184 = VECTOR ( 'NONE', #2063, 1000.000000000000114 ) ;
#13185 = PRODUCT_DEFINITION_SHAPE ( 'NONE', 'NONE',  #14486 ) ;
#13186 = FACE_OUTER_BOUND ( 'NONE', #12871, .T. ) ;
#13187 = VECTOR ( 'NONE', #6552, 1000.000000000000000 ) ;
#13188 = EDGE_CURVE ( 'NONE', #5967, #8043, #4765, .T. ) ;
#13189 = EDGE_CURVE ( 'NONE', #2673, #1985, #8260, .T. ) ;
#13190 = VERTEX_POINT ( 'NONE', #9140 ) ;
#13191 = AXIS2_PLACEMENT_3D ( 'NONE', #4563, #6726, #8 ) ;
#13192 = VERTEX_POINT ( 'NONE', #6944 ) ;
#13193 = CARTESIAN_POINT ( 'NONE',  ( -4.378301941662546604, 3.528365556573288320, -4.490643565754954381 ) ) ;
#13194 = DIRECTION ( 'NONE',  ( -0.000000000000000000, 1.000000000000000000, -0.000000000000000000 ) ) ;
#13195 = CARTESIAN_POINT ( 'NONE',  ( 88.22284556172391490, 39.57655509336063915, 33.00000000000002842 ) ) ;
#13196 = FACE_OUTER_BOUND ( 'NONE', #2229, .T. ) ;
#13198 = VECTOR ( 'NONE', #12417, 1000.000000000000000 ) ;
#13197 =( NAMED_UNIT ( * ) PLANE_ANGLE_UNIT ( ) SI_UNIT ( $, .RADIAN. ) );
#13199 = EDGE_CURVE ( 'NONE', #8916, #3067, #2644, .T. ) ;
#13200 = ORIENTED_EDGE ( 'NONE', *, *, #7390, .T. ) ;
#13201 = DIRECTION ( 'NONE',  ( 0.000000000000000000, 0.000000000000000000, 1.000000000000000000 ) ) ;
#13202 = CARTESIAN_POINT ( 'NONE',  ( 22.00000000000000711, 20.00000000000000355, -25.00000000000000000 ) ) ;
#13203 = DIRECTION ( 'NONE',  ( 0.000000000000000000, -0.000000000000000000, 1.000000000000000000 ) ) ;
#13204 = CARTESIAN_POINT ( 'NONE',  ( -108.6817075744281595, 69.57655509336026967, 3.299999999999976730 ) ) ;
#13205 = CARTESIAN_POINT ( 'NONE',  ( -108.6817075744282448, 109.5765550933602839, 0.000000000000000000 ) ) ;
#13206 = DIRECTION ( 'NONE',  ( 0.000000000000000000, 0.000000000000000000, 1.000000000000000000 ) ) ;
#13207 = FACE_OUTER_BOUND ( 'NONE', #14143, .T. ) ;
#13208 = CARTESIAN_POINT ( 'NONE',  ( -8.000000000000000000, 40.49999999999999289, 8.000000000000007105 ) ) ;
#13209 = CARTESIAN_POINT ( 'NONE',  ( 4.844570275110086754, -0.7957299432388361682, -4.000000000000002665 ) ) ;
#13210 = PRESENTATION_STYLE_ASSIGNMENT (( #11961 ) ) ;
#13211 = EDGE_CURVE ( 'NONE', #1645, #4842, #448, .T. ) ;
#13212 = CARTESIAN_POINT ( 'NONE',  ( 37.35300976710104948, 100.8957249956400375, 25.00000000000000000 ) ) ;
#13213 = VERTEX_POINT ( 'NONE', #3529 ) ;
#13214 = ORIENTED_EDGE ( 'NONE', *, *, #7682, .T. ) ;
#13215 = LINE ( 'NONE', #4219, #13750 ) ;
#13216 = CARTESIAN_POINT ( 'NONE',  ( 4.236525418537980592, -2.416953631397936064, -3.451298686683613060 ) ) ;
#13217 = ORIENTED_EDGE ( 'NONE', *, *, #6206, .T. ) ;
#13218 = DIRECTION ( 'NONE',  ( 1.000000000000000000, -2.551526159633733968E-19, -1.987661601597216239E-18 ) ) ;
#13219 = FACE_BOUND ( 'NONE', #8263, .T. ) ;
#13220 = ORIENTED_EDGE ( 'NONE', *, *, #3247, .T. ) ;
#13221 = EDGE_LOOP ( 'NONE', ( #7886, #9729, #1109, #11331, #5695 ) ) ;
#13222 = ORIENTED_EDGE ( 'NONE', *, *, #4361, .T. ) ;
#13223 = CARTESIAN_POINT ( 'NONE',  ( -3.081487911019577365E-30, 3.469446951953614189E-15, -25.03750572909319061 ) ) ;
#13224 = CARTESIAN_POINT ( 'NONE',  ( -3.177713737242648939, 47.84352126631786462, 6.443209146269483156 ) ) ;
#13225 = FACE_OUTER_BOUND ( 'NONE', #3078, .T. ) ;
#13226 = CARTESIAN_POINT ( 'NONE',  ( 6.532899837730830939, 3.469446951953614189E-15, -5.432899837730820636 ) ) ;
#13227 = EDGE_CURVE ( 'NONE', #14186, #3878, #2882, .T. ) ;
#13228 = DIRECTION ( 'NONE',  ( -1.000000000000000000, -1.665334536937734071E-16, 0.000000000000000000 ) ) ;
#13229 = VERTEX_POINT ( 'NONE', #7011 ) ;
#13230 = PRODUCT_DEFINITION ( 'UNKNOWN', '', #10836, #4573 ) ;
#13231 = SURFACE_SIDE_STYLE ('',( #10943 ) ) ;
#13232 = CARTESIAN_POINT ( 'NONE',  ( 2.450000000000000622, 0.000000000000000000, -0.3851141460153306717 ) ) ;
#13233 = FACE_OUTER_BOUND ( 'NONE', #12951, .T. ) ;
#13234 = VECTOR ( 'NONE', #3608, 999.9999999999998863 ) ;
#13235 = ORIENTED_EDGE ( 'NONE', *, *, #11095, .F. ) ;
#13236 = ORIENTED_EDGE ( 'NONE', *, *, #11457, .T. ) ;
#13237 = DIRECTION ( 'NONE',  ( 0.000000000000000000, 0.000000000000000000, -1.000000000000000000 ) ) ;
#13238 = ORIENTED_EDGE ( 'NONE', *, *, #4255, .T. ) ;
#13239 = DIRECTION ( 'NONE',  ( 0.000000000000000000, 0.000000000000000000, 1.000000000000000000 ) ) ;
#13240 = CARTESIAN_POINT ( 'NONE',  ( 60.00000000000000000, -6.123233995736768255E-16, 25.00000000000000000 ) ) ;
#13241 = CARTESIAN_POINT ( 'NONE',  ( 1.786241414228628255, 48.30187417244851389, 0.4115279878254324286 ) ) ;
#13242 = CARTESIAN_POINT ( 'NONE',  ( 22.00000000000000000, 80.00000000000000000, -25.00000000000000000 ) ) ;
#13243 = LINE ( 'NONE', #3218, #12900 ) ;
#13244 = ITEM_DEFINED_TRANSFORMATION ( 'NONE', 'NONE', #6859,  #11025 ) ;
#13245 = DIRECTION ( 'NONE',  ( 1.000000000000000000, 3.286707217423839940E-17, 2.273843122241288053E-18 ) ) ;
#13246 = CARTESIAN_POINT ( 'NONE',  ( 3.974175853610038445, -3.450041667725644690, 1.156004144284026758 ) ) ;
#13247 = ORIENTED_EDGE ( 'NONE', *, *, #10393, .F. ) ;
#13248 = EDGE_CURVE ( 'NONE', #6553, #13013, #12451, .T. ) ;
#13249 = CARTESIAN_POINT ( 'NONE',  ( 30.00229726637438432, 120.2985749985466839, 25.00000000000000000 ) ) ;
#13250 = VERTEX_POINT ( 'NONE', #7086 ) ;
#13251 = EDGE_LOOP ( 'NONE', ( #13502, #8677, #12963 ) ) ;
#13252 = DIRECTION ( 'NONE',  ( 0.000000000000000000, 0.000000000000000000, -1.000000000000000000 ) ) ;
#13253 = CIRCLE ( 'NONE', #6924, 2.500000000000002220 ) ;
#13254 = CARTESIAN_POINT ( 'NONE',  ( -5.000000000000000000, 0.4965892259340516923, -0.01450341304856382109 ) ) ;
#13255 = CARTESIAN_POINT ( 'NONE',  ( 19.99999999999999645, 57.00000000000000000, 25.00000000000000000 ) ) ;
#13256 = ORIENTED_EDGE ( 'NONE', *, *, #8946, .T. ) ;
#13257 = CARTESIAN_POINT ( 'NONE',  ( 22.00000000000000000, 70.00000000000000000, 25.00000000000000000 ) ) ;
#13258 = DIRECTION ( 'NONE',  ( 3.469446951953772885E-18, 7.771561172376088880E-16, -1.000000000000000000 ) ) ;
#13259 = EDGE_CURVE ( 'NONE', #12519, #1702, #4056, .T. ) ;
#13260 = DIRECTION ( 'NONE',  ( 0.000000000000000000, 1.000000000000000000, 0.000000000000000000 ) ) ;
#13261 = ORIENTED_EDGE ( 'NONE', *, *, #9630, .F. ) ;
#13262 = CARTESIAN_POINT ( 'NONE',  ( 1.560000000000005826, -1.732050807568885631, 0.000000000000000000 ) ) ;
#13263 = DIRECTION ( 'NONE',  ( 1.000000000000000000, 1.665334536937734071E-16, 0.000000000000000000 ) ) ;
#13264 = AXIS2_PLACEMENT_3D ( 'NONE', #5859, #3765, #9471 ) ;
#13265 = ADVANCED_FACE ( 'NONE', ( #4902 ), #4627, .F. ) ;
#13266 =( REPRESENTATION_RELATIONSHIP ('NONE','NONE', #10295, #3865 ) REPRESENTATION_RELATIONSHIP_WITH_TRANSFORMATION ( #2696 )SHAPE_REPRESENTATION_RELATIONSHIP( ) );
#13267 = DIRECTION ( 'NONE',  ( 0.000000000000000000, 0.000000000000000000, 1.000000000000000000 ) ) ;
#13268 = VERTEX_POINT ( 'NONE', #6881 ) ;
#13269 = VECTOR ( 'NONE', #5385, 1000.000000000000000 ) ;
#13270 = CARTESIAN_POINT ( 'NONE',  ( -0.5636734750058277621, -4.293365120987121308, -3.231543764079341408 ) ) ;
#13271 = EDGE_CURVE ( 'NONE', #13079, #4424, #12733, .T. ) ;
#13272 = CARTESIAN_POINT ( 'NONE',  ( 4.851472949720941230, -4.233901974057260986, -0.6666666666666652974 ) ) ;
#13273 = CARTESIAN_POINT ( 'NONE',  ( 4.939003118777821832, -2.662716476701425083, 3.388039776202045328 ) ) ;
#13274 = DIRECTION ( 'NONE',  ( -0.000000000000000000, -0.000000000000000000, -1.000000000000000000 ) ) ;
#13275 = LINE ( 'NONE', #2072, #13583 ) ;
#13276 = PLANE ( 'NONE',  #8868 ) ;
#13277 = EDGE_CURVE ( 'NONE', #4680, #13498, #5981, .T. ) ;
#13278 = AXIS2_PLACEMENT_3D ( 'NONE', #2596, #10496, #4792 ) ;
#13279 = CARTESIAN_POINT ( 'NONE',  ( 53.99999999999997868, -1.347111479062091166E-15, -25.00000000000000000 ) ) ;
#13280 = CIRCLE ( 'NONE', #10223, 3.200000000000000622 ) ;
#13281 = EDGE_LOOP ( 'NONE', ( #2583, #6717, #14309, #9734 ) ) ;
#13282 = ORIENTED_EDGE ( 'NONE', *, *, #14119, .F. ) ;
#13283 = CARTESIAN_POINT ( 'NONE',  ( -2.501150643247835315E-15, -20.42344490663947809, 33.00000000000002842 ) ) ;
#13284 = ORIENTED_EDGE ( 'NONE', *, *, #3619, .F. ) ;
#13285 = LINE ( 'NONE', #4444, #2282 ) ;
#13286 = FACE_OUTER_BOUND ( 'NONE', #8669, .T. ) ;
#13287 = CONICAL_SURFACE ( 'NONE', #5771, 4.000000000000000000, 0.8911886515913775009 ) ;
#13288 = VERTEX_POINT ( 'NONE', #7154 ) ;
#13289 = EDGE_CURVE ( 'NONE', #4994, #10243, #62, .T. ) ;
#13290 = CONICAL_SURFACE ( 'NONE', #2531, 3.499999999999999112, 1.047197551196600296 ) ;
#13291 = ORIENTED_EDGE ( 'NONE', *, *, #2908, .T. ) ;
#13292 = CARTESIAN_POINT ( 'NONE',  ( 4.071447262713911996, 2.020725942163681399, -3.499999999999996003 ) ) ;
#13293 = CARTESIAN_POINT ( 'NONE',  ( 3.973110223767151616, 2.262797354954571809E-11, 3.565797985667430225 ) ) ;
#13294 = CARTESIAN_POINT ( 'NONE',  ( 22.00000000000000711, 17.00000000000000000, -25.00000000000000000 ) ) ;
#13295 = DIRECTION ( 'NONE',  ( 1.000000000000000000, 0.000000000000000000, 0.000000000000000000 ) ) ;
#13296 = PRODUCT_DEFINITION_SHAPE ( 'NONE', 'NONE',  #14487 ) ;
#13297 = FACE_OUTER_BOUND ( 'NONE', #2393, .T. ) ;
#13298 = DIRECTION ( 'NONE',  ( 1.000000000000000000, -0.000000000000000000, -0.000000000000000000 ) ) ;
#13299 = SURFACE_STYLE_USAGE ( .BOTH. , #13231 ) ;
#13300 = CARTESIAN_POINT ( 'NONE',  ( 4.872568031907690056, 3.922980182067759891, -1.349977486297356144 ) ) ;
#13301 = COLOUR_RGB ( '', 0.09019608, 0.27058824, 0.51372549) ;
#13302 = DIRECTION ( 'NONE',  ( -1.000000000000000000, 0.000000000000000000, 0.000000000000000000 ) ) ;
#13303 = ORIENTED_EDGE ( 'NONE', *, *, #2723, .T. ) ;
#13304 = ORIENTED_EDGE ( 'NONE', *, *, #5849, .F. ) ;
#13305 = EDGE_CURVE ( 'NONE', #10136, #10163, #2313, .T. ) ;
#13306 = ORIENTED_EDGE ( 'NONE', *, *, #1983, .T. ) ;
#13307 = ORIENTED_EDGE ( 'NONE', *, *, #161, .F. ) ;
#13308 = DIRECTION ( 'NONE',  ( 1.000000000000000000, 1.224646799147353454E-16, -0.000000000000000000 ) ) ;
#13309 = CARTESIAN_POINT ( 'NONE',  ( 4.158921444904712494, -2.089933220600059371, -3.499999999999992895 ) ) ;
#13310 = DIRECTION ( 'NONE',  ( 0.9701425001453319874, 0.2425356250363330801, 0.000000000000000000 ) ) ;
#13311 = DIRECTION ( 'NONE',  ( 1.000000000000000000, 1.665334536937734071E-16, 0.000000000000000000 ) ) ;
#13312 = CARTESIAN_POINT ( 'NONE',  ( 0.000000000000000000, 0.000000000000000000, 0.000000000000000000 ) ) ;
#13313 = DIRECTION ( 'NONE',  ( 0.000000000000000000, -1.000000000000000000, 0.000000000000000000 ) ) ;
#13314 = VECTOR ( 'NONE', #11621, 1000.000000000000000 ) ;
#13315 = ITEM_DEFINED_TRANSFORMATION ( 'NONE', 'NONE', #1255,  #11025 ) ;
#13316 = DIRECTION ( 'NONE',  ( -0.000000000000000000, -0.000000000000000000, 1.000000000000000000 ) ) ;
#13317 = CARTESIAN_POINT ( 'NONE',  ( 4.124214193018061358, 2.028338413290956765, -3.513185186763553070 ) ) ;
#13318 = ORIENTED_EDGE ( 'NONE', *, *, #8768, .F. ) ;
#13319 = LINE ( 'NONE', #5612, #2892 ) ;
#13320 = ORIENTED_EDGE ( 'NONE', *, *, #9596, .T. ) ;
#13321 = VECTOR ( 'NONE', #13767, 1000.000000000000000 ) ;
#13322 = ORIENTED_EDGE ( 'NONE', *, *, #9395, .F. ) ;
#13323 = VERTEX_POINT ( 'NONE', #13559 ) ;
#13324 = EDGE_CURVE ( 'NONE', #13714, #6682, #5196, .T. ) ;
#13325 = EDGE_CURVE ( 'NONE', #2033, #12126, #8408, .T. ) ;
#13326 = VECTOR ( 'NONE', #8638, 1000.000000000000114 ) ;
#13327 = ORIENTED_EDGE ( 'NONE', *, *, #6509, .T. ) ;
#13328 = ORIENTED_EDGE ( 'NONE', *, *, #5413, .F. ) ;
#13329 = PLANE ( 'NONE',  #12579 ) ;
#13330 = LINE ( 'NONE', #5621, #12671 ) ;
#13331 = FACE_OUTER_BOUND ( 'NONE', #10966, .T. ) ;
#13332 = DIRECTION ( 'NONE',  ( 0.000000000000000000, -1.224646799147353207E-16, 1.000000000000000000 ) ) ;
#13333 = ADVANCED_FACE ( 'NONE', ( #14208 ), #11934, .F. ) ;
#13334 = ORIENTED_EDGE ( 'NONE', *, *, #13104, .F. ) ;
#13335 = DIRECTION ( 'NONE',  ( 0.000000000000000000, 0.000000000000000000, -1.000000000000000000 ) ) ;
#13336 = CARTESIAN_POINT ( 'NONE',  ( 5.000000000000001776, 2.886751345948127767, -6.000000000000005329 ) ) ;
#13337 =( NAMED_UNIT ( * ) PLANE_ANGLE_UNIT ( ) SI_UNIT ( $, .RADIAN. ) );
#13338 = CARTESIAN_POINT ( 'NONE',  ( 118.6817075744280174, -30.42344490663937506, 33.00000000000002842 ) ) ;
#13339 = ORIENTED_EDGE ( 'NONE', *, *, #1776, .T. ) ;
#13340 = ORIENTED_EDGE ( 'NONE', *, *, #12426, .T. ) ;
#13341 = CARTESIAN_POINT ( 'NONE',  ( 76.68170757442804586, 59.57655509336061073, -25.00000000000000000 ) ) ;
#13342 = CARTESIAN_POINT ( 'NONE',  ( 76.68170757442801744, 144.5765550933605823, -33.00000000000000000 ) ) ;
#13343 = DIRECTION ( 'NONE',  ( -1.000000000000000000, 0.000000000000000000, 0.000000000000000000 ) ) ;
#13344 = STYLED_ITEM ( 'NONE', ( #7062 ), #11564 ) ;
#13345 = EDGE_CURVE ( 'NONE', #7747, #7417, #1908, .T. ) ;
#13346 = CIRCLE ( 'NONE', #12400, 3.299999999999983391 ) ;
#13347 = EDGE_CURVE ( 'NONE', #1341, #4098, #1450, .T. ) ;
#13348 = CARTESIAN_POINT ( 'NONE',  ( 108.6817075744280459, 189.5765550933606107, -106.9999999999999858 ) ) ;
#13349 = PRODUCT_DEFINITION_CONTEXT ( 'detailed design', #8847, 'design' ) ;
#13350 = CARTESIAN_POINT ( 'NONE',  ( 4.942464816486591417, -4.274687029205462174, 0.5960248789590811835 ) ) ;
#13351 = DIRECTION ( 'NONE',  ( 1.000000000000000000, 0.000000000000000000, 0.000000000000000000 ) ) ;
#13352 = ADVANCED_FACE ( 'NONE', ( #14069 ), #675, .F. ) ;
#13353 = CARTESIAN_POINT ( 'NONE',  ( 4.988724804725785944, -2.309401076758511806, -3.999999999999989786 ) ) ;
#13354 = SHAPE_REPRESENTATION_RELATIONSHIP ( 'NONE' , 'NONE' ,  #7856, #13112 ) ;
#13355 = B_SPLINE_CURVE_WITH_KNOTS ( 'NONE', 3,
 ( #11036, #1156, #6563, #863, #1012, #5609 ),
 .UNSPECIFIED., .F., .F.,
 ( 4, 2, 4 ),
 ( 0.000000000000000000, 0.0002095117440854733380, 0.0004190234881709466760 ),
 .UNSPECIFIED. ) ;
#13356 = AXIS2_PLACEMENT_3D ( 'NONE', #1664, #6113, #12864 ) ;
#13357 = CARTESIAN_POINT ( 'NONE',  ( 5.035982117295126237, 2.314736229921496413, 4.009240756344441436 ) ) ;
#13358 = ORIENTED_EDGE ( 'NONE', *, *, #2358, .F. ) ;
#13359 = ORIENTED_EDGE ( 'NONE', *, *, #10049, .T. ) ;
#13360 = CARTESIAN_POINT ( 'NONE',  ( 2.750000000000002665, 0.000000000000000000, 0.000000000000000000 ) ) ;
#13361 = EDGE_CURVE ( 'NONE', #5931, #10136, #11195, .T. ) ;
#13362 = VECTOR ( 'NONE', #13137, 1000.000000000000000 ) ;
#13363 = SURFACE_STYLE_FILL_AREA ( #4365 ) ;
#13364 = VERTEX_POINT ( 'NONE', #2796 ) ;
#13365 = CARTESIAN_POINT ( 'NONE',  ( 0.000000000000000000, 19.49999999999999645, 8.000000000000007105 ) ) ;
#13366 = CARTESIAN_POINT ( 'NONE',  ( 0.3572655899081733644, 2.309401076758511806, 3.999999999999989786 ) ) ;
#13367 = ORIENTED_EDGE ( 'NONE', *, *, #11385, .T. ) ;
#13368 = EDGE_CURVE ( 'NONE', #6300, #1350, #10689, .T. ) ;
#13369 = EDGE_CURVE ( 'NONE', #79, #6673, #9637, .T. ) ;
#13370 = VECTOR ( 'NONE', #7227, 1000.000000000000000 ) ;
#13371 = AXIS2_PLACEMENT_3D ( 'NONE', #11789, #5333, #3019 ) ;
#13372 = EDGE_LOOP ( 'NONE', ( #3023, #5198, #9626, #11194, #11147 ) ) ;
#13373 = CARTESIAN_POINT ( 'NONE',  ( 60.00000000000000000, -6.123233995736768255E-16, 25.00000000000000000 ) ) ;
#13374 = DIRECTION ( 'NONE',  ( 0.000000000000000000, -1.000000000000000000, 0.000000000000000000 ) ) ;
#13375 = EDGE_CURVE ( 'NONE', #1702, #12519, #1700, .T. ) ;
#13376 = CARTESIAN_POINT ( 'NONE',  ( 4.055492966679507205, -2.385006769472553856, -3.005124364834288908 ) ) ;
#13377 = DIRECTION ( 'NONE',  ( -0.000000000000000000, -1.000000000000000000, 0.000000000000000000 ) ) ;
#13378 = CARTESIAN_POINT ( 'NONE',  ( 0.000000000000000000, 4.041451884327390331, 0.000000000000000000 ) ) ;
#13379 = DIRECTION ( 'NONE',  ( 1.000000000000000000, 3.286707217423839940E-17, 2.273843122241288053E-18 ) ) ;
#13380 = ORIENTED_EDGE ( 'NONE', *, *, #14047, .T. ) ;
#13381 = FILL_AREA_STYLE ('',( #7718 ) ) ;
#13382 = DIRECTION ( 'NONE',  ( 0.2425356250363328581, -0.9701425001453318764, -0.000000000000000000 ) ) ;
#13383 = EDGE_CURVE ( 'NONE', #6697, #1128, #2848, .T. ) ;
#13384 = VECTOR ( 'NONE', #6725, 1000.000000000000000 ) ;
#13385 = VECTOR ( 'NONE', #13316, 1000.000000000000000 ) ;
#13386 = CARTESIAN_POINT ( 'NONE',  ( 4.180345304246193550, 4.135116856707387711, -0.02129519942690456108 ) ) ;
#13387 = EDGE_LOOP ( 'NONE', ( #8191, #4087, #12441, #11259 ) ) ;
#13388 = ORIENTED_EDGE ( 'NONE', *, *, #7881, .T. ) ;
#13389 = CARTESIAN_POINT ( 'NONE',  ( 5.103531824934171013, 2.354098498486459246, -4.077418205400141105 ) ) ;
#13390 = AXIS2_PLACEMENT_3D ( 'NONE', #14245, #1952, #11759 ) ;
#13391 = ORIENTED_EDGE ( 'NONE', *, *, #9309, .F. ) ;
#13392 = CARTESIAN_POINT ( 'NONE',  ( 3.878104551856469850, -0.7018542299766717951, -3.499999999999992895 ) ) ;
#13393 = AXIS2_PLACEMENT_3D ( 'NONE', #6588, #7678, #13487 ) ;
#13394 = CARTESIAN_POINT ( 'NONE',  ( -4.999999999999999112, -2.426004080355347980, -0.4213009713786298738 ) ) ;
#13395 = ORIENTED_EDGE ( 'NONE', *, *, #7252, .F. ) ;
#13396 = CARTESIAN_POINT ( 'NONE',  ( 71.80728622811317052, -17.99808865627607801, 28.00000000000000000 ) ) ;
#13397 = LINE ( 'NONE', #10828, #6718 ) ;
#13398 = ORIENTED_EDGE ( 'NONE', *, *, #9151, .F. ) ;
#13399 = CARTESIAN_POINT ( 'NONE',  ( 2.949999999999994404, 3.061616997868382155E-16, -2.499999999999999112 ) ) ;
#13400 = ITEM_DEFINED_TRANSFORMATION ( 'NONE', 'NONE', #2423,  #11025 ) ;
#13401 = CARTESIAN_POINT ( 'NONE',  ( 3.999999999999998224, 1.658584703716829312, -3.231554742509630707 ) ) ;
#13402 = EDGE_CURVE ( 'NONE', #12702, #9280, #760, .T. ) ;
#13403 = CARTESIAN_POINT ( 'NONE',  ( 5.102759246810640192, -4.706121570500099160, 4.163336342344337027E-14 ) ) ;
#13404 = AXIS2_PLACEMENT_3D ( 'NONE', #13439, #12393, #12257 ) ;
#13405 = CARTESIAN_POINT ( 'NONE',  ( 0.000000000000000000, 0.000000000000000000, 0.000000000000000000 ) ) ;
#13407 = ORIENTED_EDGE ( 'NONE', *, *, #12122, .T. ) ;
#13406 = AXIS2_PLACEMENT_3D ( 'NONE', #4129, #1917, #5201 ) ;
#13408 = ORIENTED_EDGE ( 'NONE', *, *, #9070, .T. ) ;
#13409 = LINE ( 'NONE', #6427, #5476 ) ;
#13410 = ORIENTED_EDGE ( 'NONE', *, *, #6509, .F. ) ;
#13411 = CARTESIAN_POINT ( 'NONE',  ( 31.41872415839353039, 143.5561596226024790, 28.00000000000000000 ) ) ;
#13412 = DIRECTION ( 'NONE',  ( 0.000000000000000000, 0.000000000000000000, -1.000000000000000000 ) ) ;
#13413 = PLANE ( 'NONE',  #13103 ) ;
#13414 = DIRECTION ( 'NONE',  ( -1.000000000000000000, 1.892425610156516875E-16, 0.000000000000000000 ) ) ;
#13415 = VECTOR ( 'NONE', #11874, 1000.000000000000000 ) ;
#13416 = VERTEX_POINT ( 'NONE', #7233 ) ;
#13417 = CARTESIAN_POINT ( 'NONE',  ( 22.00000000000000355, 37.00000000000000711, 25.00000000000000000 ) ) ;
#13418 = DIRECTION ( 'NONE',  ( 0.000000000000000000, 0.000000000000000000, -1.000000000000000000 ) ) ;
#13419 = DIRECTION ( 'NONE',  ( 0.000000000000000000, 0.000000000000000000, -1.000000000000000000 ) ) ;
#13420 = EDGE_CURVE ( 'NONE', #14288, #11273, #3966, .T. ) ;
#13421 = CYLINDRICAL_SURFACE ( 'NONE', #6570, 2.100000000000000977 ) ;
#13422 = ORIENTED_EDGE ( 'NONE', *, *, #4661, .T. ) ;
#13423 = PRODUCT_RELATED_PRODUCT_CATEGORY ( 'part', '', ( #63 ) ) ;
#13424 = EDGE_CURVE ( 'NONE', #11445, #6344, #2626, .T. ) ;
#13425 = CARTESIAN_POINT ( 'NONE',  ( -2.068360682592150557, -4.579334095020470841, -0.01465562841809295996 ) ) ;
#13426 = CARTESIAN_POINT ( 'NONE',  ( 39.77836601746437850, 91.19429999418670718, 25.00000000000000000 ) ) ;
#13427 = DIRECTION ( 'NONE',  ( 1.000000000000000000, 1.927470528863118802E-16, 0.000000000000000000 ) ) ;
#13428 = EDGE_LOOP ( 'NONE', ( #12981, #3189, #10612, #14191 ) ) ;
#13429 = PRODUCT_DEFINITION_SHAPE ( 'NONE', 'NONE',  #14484 ) ;
#13430 = CARTESIAN_POINT ( 'NONE',  ( 23.40000000000000213, 29.99999999999999645, -34.50000000000000000 ) ) ;
#13431 = VECTOR ( 'NONE', #8614, 999.9999999999998863 ) ;
#13432 = DIRECTION ( 'NONE',  ( -4.406877377903809255E-17, 1.000000000000000000, 0.000000000000000000 ) ) ;
#13433 = DIRECTION ( 'NONE',  ( 1.000000000000000000, -0.000000000000000000, -0.000000000000000000 ) ) ;
#13434 = PLANE ( 'NONE',  #4457 ) ;
#13435 = CARTESIAN_POINT ( 'NONE',  ( 5.056385618527004411, 2.321455725013347848, 4.020879263244750312 ) ) ;
#13436 = VERTEX_POINT ( 'NONE', #3022 ) ;
#13437 = DIRECTION ( 'NONE',  ( -1.000000000000000000, -8.619211990076296383E-16, 0.000000000000000000 ) ) ;
#13438 = VERTEX_POINT ( 'NONE', #6059 ) ;
#13439 = CARTESIAN_POINT ( 'NONE',  ( 0.000000000000000000, 0.000000000000000000, 0.000000000000000000 ) ) ;
#13440 = ORIENTED_EDGE ( 'NONE', *, *, #886, .F. ) ;
#13441 = EDGE_LOOP ( 'NONE', ( #12664, #12741, #6966, #9621 ) ) ;
#13442 = CARTESIAN_POINT ( 'NONE',  ( -1.647413659512543482, 4.822367972110034096, -0.05822226285683312907 ) ) ;
#13443 = DIRECTION ( 'NONE',  ( -1.000000000000000000, 0.000000000000000000, 0.000000000000000000 ) ) ;
#13444 = DIRECTION ( 'NONE',  ( 0.000000000000000000, 1.000000000000000000, 0.000000000000000000 ) ) ;
#13445 = CARTESIAN_POINT ( 'NONE',  ( -2.500000000000016875, -4.330127018922186544, 0.000000000000000000 ) ) ;
#13446 = SURFACE_STYLE_FILL_AREA ( #9241 ) ;
#13447 = DIRECTION ( 'NONE',  ( 1.000000000000000000, 3.286707217423839940E-17, 2.273843122241288053E-18 ) ) ;
#13448 = CARTESIAN_POINT ( 'NONE',  ( 4.872568031907691832, 3.130604888704443756, 2.722411753064904794 ) ) ;
#13449 =( LENGTH_UNIT ( ) NAMED_UNIT ( * ) SI_UNIT ( .MILLI., .METRE. ) );
#13450 = EDGE_CURVE ( 'NONE', #3640, #10543, #3577, .T. ) ;
#13451 = ORIENTED_EDGE ( 'NONE', *, *, #9520, .F. ) ;
#13452 = DIRECTION ( 'NONE',  ( 0.000000000000000000, 0.000000000000000000, -1.000000000000000000 ) ) ;
#13453 = DIRECTION ( 'NONE',  ( 0.000000000000000000, 0.000000000000000000, -1.000000000000000000 ) ) ;
#13454 = ORIENTED_EDGE ( 'NONE', *, *, #6273, .F. ) ;
#13455 = ORIENTED_EDGE ( 'NONE', *, *, #8544, .T. ) ;
#13456 = ORIENTED_EDGE ( 'NONE', *, *, #13522, .F. ) ;
#13457 = CARTESIAN_POINT ( 'NONE',  ( -3.081487911019577365E-30, 3.469446951953614189E-15, -5.974599999999997024 ) ) ;
#13458 = EDGE_CURVE ( 'NONE', #4904, #5824, #11709, .T. ) ;
#13459 = EDGE_LOOP ( 'NONE', ( #9501, #3679, #13217, #597 ) ) ;
#13460 = CARTESIAN_POINT ( 'NONE',  ( 3.948111298834958482, -0.6968132764982380989, -3.499999999999837019 ) ) ;
#13461 = CARTESIAN_POINT ( 'NONE',  ( 49.40514726928103073, 42.68717498692012668, 25.00000000000000000 ) ) ;
#13462 = LINE ( 'NONE', #9109, #5355 ) ;
#13463 = DIRECTION ( 'NONE',  ( 1.000000000000000000, 1.665334536937734071E-16, 0.000000000000000000 ) ) ;
#13464 = CARTESIAN_POINT ( 'NONE',  ( 32.50229726637438432, 120.2985749985466839, -25.00000000000000000 ) ) ;
#13465 = EDGE_CURVE ( 'NONE', #4572, #937, #10109, .T. ) ;
#13466 = LINE ( 'NONE', #3436, #5617 ) ;
#13467 = DIRECTION ( 'NONE',  ( -1.000000000000000000, 0.000000000000000000, 0.000000000000000000 ) ) ;
#13468 = CARTESIAN_POINT ( 'NONE',  ( 4.124214193018059582, -2.028338413290955877, 3.513185186763558843 ) ) ;
#13469 = B_SPLINE_CURVE_WITH_KNOTS ( 'NONE', 3,
 ( #7276, #11753, #8146, #1731, #639 ),
 .UNSPECIFIED., .F., .F.,
 ( 4, 1, 4 ),
 ( 0.000000000000000000, 0.002309401076758505790, 0.004618802153517011580 ),
 .UNSPECIFIED. ) ;
#13470 = ORIENTED_EDGE ( 'NONE', *, *, #118, .T. ) ;
#13471 = ORIENTED_EDGE ( 'NONE', *, *, #9598, .T. ) ;
#13472 = DIRECTION ( 'NONE',  ( 1.000000000000000000, -0.000000000000000000, -0.000000000000000000 ) ) ;
#13473 = ADVANCED_FACE ( 'NONE', ( #10896 ), #12289, .T. ) ;
#13474 = ORIENTED_EDGE ( 'NONE', *, *, #3923, .T. ) ;
#13475 = CARTESIAN_POINT ( 'NONE',  ( 4.817220356105922363, -3.279784343982821593, -4.566919140436432656 ) ) ;
#13476 = CARTESIAN_POINT ( 'NONE',  ( -3.081487911019577365E-30, 3.469446951953614189E-15, -6.000000000000005329 ) ) ;
#13477 = PRESENTATION_STYLE_ASSIGNMENT (( #12571 ) ) ;
#13478 = DIRECTION ( 'NONE',  ( -0.000000000000000000, -1.000000000000000000, 0.000000000000000000 ) ) ;
#13479 = ORIENTED_EDGE ( 'NONE', *, *, #10244, .F. ) ;
#13480 = PLANE ( 'NONE',  #1550 ) ;
#13481 = DIRECTION ( 'NONE',  ( 1.927470528863118802E-16, -1.000000000000000000, -0.000000000000000000 ) ) ;
#13482 = CARTESIAN_POINT ( 'NONE',  ( 125.4817075744280572, 109.5765550933604828, 1.102184477801737558E-14 ) ) ;
#13483 = DIRECTION ( 'NONE',  ( 0.000000000000000000, 0.000000000000000000, 1.000000000000000000 ) ) ;
#13484 = VERTEX_POINT ( 'NONE', #2199 ) ;
#13485 = ORIENTED_EDGE ( 'NONE', *, *, #13807, .T. ) ;
#13486 = CARTESIAN_POINT ( 'NONE',  ( 20.00000000000000000, -5.510910596163090344E-15, 25.00000000000000000 ) ) ;
#13487 = DIRECTION ( 'NONE',  ( 1.000000000000000000, 0.000000000000000000, 0.000000000000000000 ) ) ;
#13488 = ORIENTED_EDGE ( 'NONE', *, *, #11548, .T. ) ;
#13489 = VECTOR ( 'NONE', #10638, 1000.000000000000000 ) ;
#13490 = ORIENTED_EDGE ( 'NONE', *, *, #12218, .F. ) ;
#13491 = EDGE_CURVE ( 'NONE', #5215, #1341, #13319, .T. ) ;
#13492 = EDGE_CURVE ( 'NONE', #12253, #4722, #1465, .T. ) ;
#13493 = CARTESIAN_POINT ( 'NONE',  ( 1.560000000000005826, -0.8660254037844428154, 1.500000000000001332 ) ) ;
#13494 = CARTESIAN_POINT ( 'NONE',  ( 40.00000000000000711, 80.00000000000000000, -25.00000000000000000 ) ) ;
#13495 = CARTESIAN_POINT ( 'NONE',  ( 71.80728622811317052, -17.99808865627607801, -28.00000000000000000 ) ) ;
#13496 = DIRECTION ( 'NONE',  ( -1.000000000000000000, 0.000000000000000000, 0.000000000000000000 ) ) ;
#13497 = ORIENTED_EDGE ( 'NONE', *, *, #13733, .T. ) ;
#13498 = VERTEX_POINT ( 'NONE', #10964 ) ;
#13499 = CARTESIAN_POINT ( 'NONE',  ( 0.000000000000000000, -30.42444490663959300, -37.00000000000003553 ) ) ;
#13500 = AXIS2_PLACEMENT_3D ( 'NONE', #10064, #6545, #9997 ) ;
#13501 = AXIS2_PLACEMENT_3D ( 'NONE', #11764, #648, #9261 ) ;
#13502 = ORIENTED_EDGE ( 'NONE', *, *, #4516, .F. ) ;
#13503 = FACE_OUTER_BOUND ( 'NONE', #7001, .T. ) ;
#13504 = ORIENTED_EDGE ( 'NONE', *, *, #5664, .T. ) ;
#13505 = PRODUCT ( 'socket button head screw_iso_ISO 7380 - M5 x 25 - 25N', 'socket button head screw_iso_ISO 7380 - M5 x 25 - 25N', '', ( #14137 ) ) ;
#13506 = PLANE ( 'NONE',  #6627 ) ;
#13507 = CARTESIAN_POINT ( 'NONE',  ( 3.806834918298612536, -3.031088913245542305, 1.750000000000002442 ) ) ;
#13508 = CIRCLE ( 'NONE', #11162, 5.499999999999984013 ) ;
#13509 = CARTESIAN_POINT ( 'NONE',  ( -140.0000000000003411, 199.5765550933606107, -132.0000000000000000 ) ) ;
#13510 = CARTESIAN_POINT ( 'NONE',  ( -108.6817075744279890, 189.5765550933605823, -106.9999999999999858 ) ) ;
#13511 = CARTESIAN_POINT ( 'NONE',  ( 4.071447262713911996, 4.041451884327390331, 0.000000000000000000 ) ) ;
#13512 = CARTESIAN_POINT ( 'NONE',  ( 4.175813232069169878, 4.122719923832743660, 0.000000000000000000 ) ) ;
#13513 = FACE_OUTER_BOUND ( 'NONE', #8030, .T. ) ;
#13514 = ORIENTED_EDGE ( 'NONE', *, *, #5650, .F. ) ;
#13515 = CARTESIAN_POINT ( 'NONE',  ( 21.68170757442808849, 141.2731697022877313, 23.00000000000000000 ) ) ;
#13516 = CARTESIAN_POINT ( 'NONE',  ( 4.033901012036112732, 2.321269032828268131, 2.979444097106787481 ) ) ;
#13517 = AXIS2_PLACEMENT_3D ( 'NONE', #13928, #10478, #7098 ) ;
#13518 = ORIENTED_EDGE ( 'NONE', *, *, #1647, .T. ) ;
#13519 = CIRCLE ( 'NONE', #4851, 4.999999999999988454 ) ;
#13520 = VERTEX_POINT ( 'NONE', #6711 ) ;
#13521 = ORIENTED_EDGE ( 'NONE', *, *, #7869, .T. ) ;
#13522 = EDGE_CURVE ( 'NONE', #815, #10977, #3224, .T. ) ;
#13523 = ORIENTED_EDGE ( 'NONE', *, *, #8473, .T. ) ;
#13524 = ADVANCED_FACE ( 'NONE', ( #13186 ), #9879, .T. ) ;
#13525 = DIRECTION ( 'NONE',  ( -1.000000000000000000, -1.665334536937734071E-16, 0.000000000000000000 ) ) ;
#13526 = ORIENTED_EDGE ( 'NONE', *, *, #12112, .T. ) ;
#13527 = LINE ( 'NONE', #6700, #12858 ) ;
#13528 = CARTESIAN_POINT ( 'NONE',  ( 5.000000000000001776, 3.083561708551495695, -4.589114193688893728 ) ) ;
#13529 = EDGE_CURVE ( 'NONE', #3422, #11659, #4067, .T. ) ;
#13530 = CARTESIAN_POINT ( 'NONE',  ( -3.065261730689029740, 7.410293710401353984, 8.000000000000007105 ) ) ;
#13531 = DIRECTION ( 'NONE',  ( -1.000000000000000000, 0.000000000000000000, 0.000000000000000000 ) ) ;
#13532 = AXIS2_PLACEMENT_3D ( 'NONE', #12403, #2380, #2903 ) ;
#13533 = EDGE_CURVE ( 'NONE', #6911, #8895, #3822, .T. ) ;
#13534 = ITEM_DEFINED_TRANSFORMATION ( 'NONE', 'NONE', #12967,  #11025 ) ;
#13535 = LINE ( 'NONE', #5961, #14062 ) ;
#13536 = CARTESIAN_POINT ( 'NONE',  ( 5.076540720129292694, -4.661016483905897623, -1.387629536817191694E-14 ) ) ;
#13537 = EDGE_CURVE ( 'NONE', #5687, #10580, #11052, .T. ) ;
#13538 = VERTEX_POINT ( 'NONE', #7739 ) ;
#13539 = VERTEX_POINT ( 'NONE', #13249 ) ;
#13540 = VECTOR ( 'NONE', #9416, 1000.000000000000000 ) ;
#13541 = EDGE_CURVE ( 'NONE', #73, #5531, #10013, .T. ) ;
#13542 = EDGE_LOOP ( 'NONE', ( #8410, #3857 ) ) ;
#13543 = CARTESIAN_POINT ( 'NONE',  ( -2.807096675500548866, 3.225959780909076535, -3.202509183706246709 ) ) ;
#13544 = ORIENTED_EDGE ( 'NONE', *, *, #6182, .T. ) ;
#13545 = EDGE_CURVE ( 'NONE', #11937, #1484, #7815, .T. ) ;
#13546 = ORIENTED_EDGE ( 'NONE', *, *, #10866, .T. ) ;
#13547 = DIRECTION ( 'NONE',  ( 1.000000000000000000, 1.665334536937734071E-16, 0.000000000000000000 ) ) ;
#13548 = CARTESIAN_POINT ( 'NONE',  ( 62.10586122665987574, -20.42344490663940704, 25.00000000000000000 ) ) ;
#13549 = CARTESIAN_POINT ( 'NONE',  ( -5.000000000000000000, -3.083558758346089945, -4.589113630813312028 ) ) ;
#13550 = CARTESIAN_POINT ( 'NONE',  ( 3.355112389629170355, -2.681727112203175167, -0.2256878752776822483 ) ) ;
#13551 = ORIENTED_EDGE ( 'NONE', *, *, #6801, .F. ) ;
#13552 = DIRECTION ( 'NONE',  ( 0.000000000000000000, 0.000000000000000000, -1.000000000000000000 ) ) ;
#13553 = DIRECTION ( 'NONE',  ( 0.000000000000000000, 0.000000000000000000, 1.000000000000000000 ) ) ;
#13554 = LINE ( 'NONE', #219, #2373 ) ;
#13555 = ORIENTED_EDGE ( 'NONE', *, *, #12821, .F. ) ;
#13556 = CIRCLE ( 'NONE', #8391, 2.054999999999999716 ) ;
#13557 = ORIENTED_EDGE ( 'NONE', *, *, #1469, .F. ) ;
#13558 = EDGE_CURVE ( 'NONE', #12991, #8503, #14350, .T. ) ;
#13559 = CARTESIAN_POINT ( 'NONE',  ( 79.68170757442804586, 124.5765550933606249, -25.00000000000000000 ) ) ;
#13560 = AXIS2_PLACEMENT_3D ( 'NONE', #2709, #6130, #3813 ) ;
#13561 = VERTEX_POINT ( 'NONE', #5479 ) ;
#13562 = EDGE_LOOP ( 'NONE', ( #3264, #8741, #637, #608 ) ) ;
#13563 = EDGE_CURVE ( 'NONE', #3893, #4578, #11282, .T. ) ;
#13564 = AXIS2_PLACEMENT_3D ( 'NONE', #10677, #2939, #664 ) ;
#13565 = PLANE ( 'NONE',  #1296 ) ;
#13566 = FACE_OUTER_BOUND ( 'NONE', #13281, .T. ) ;
#13567 = FILL_AREA_STYLE ('',( #231 ) ) ;
#13568 = EDGE_LOOP ( 'NONE', ( #9102, #14352, #2731, #5053 ) ) ;
#13569 = ORIENTED_EDGE ( 'NONE', *, *, #6189, .T. ) ;
#13570 = CYLINDRICAL_SURFACE ( 'NONE', #4179, 2.500000000000002220 ) ;
#13571 = EDGE_CURVE ( 'NONE', #8264, #172, #9443, .T. ) ;
#13572 = FILL_AREA_STYLE_COLOUR ( '', #976 ) ;
#13573 = AXIS2_PLACEMENT_3D ( 'NONE', #5954, #11318, #11380 ) ;
#13574 = VERTEX_POINT ( 'NONE', #12692 ) ;
#13575 = CARTESIAN_POINT ( 'NONE',  ( 1.734723475976807094E-14, 35.49999999999996447, 8.000000000000007105 ) ) ;
#13576 = ORIENTED_EDGE ( 'NONE', *, *, #6576, .T. ) ;
#13577 = CARTESIAN_POINT ( 'NONE',  ( 22.00000000000000355, 40.00000000000000711, -25.00000000000000000 ) ) ;
#13578 = CARTESIAN_POINT ( 'NONE',  ( 25.90000000000000213, 29.99999999999999645, 25.00000000000000000 ) ) ;
#13579 = AXIS2_PLACEMENT_3D ( 'NONE', #3387, #12300, #9806 ) ;
#13580 = DIRECTION ( 'NONE',  ( 8.138903065828892551E-32, -1.000000000000000000, -7.771561172376088880E-16 ) ) ;
#13581 = MECHANICAL_DESIGN_GEOMETRIC_PRESENTATION_REPRESENTATION (  '', ( #11223 ), #487 ) ;
#13582 = CARTESIAN_POINT ( 'NONE',  ( 139.9999999999996874, 189.5765550933606107, -132.0000000000000000 ) ) ;
#13583 = VECTOR ( 'NONE', #3114, 1000.000000000000000 ) ;
#13584 =( LENGTH_UNIT ( ) NAMED_UNIT ( * ) SI_UNIT ( .MILLI., .METRE. ) );
#13585 = CARTESIAN_POINT ( 'NONE',  ( -2.085819415614008699E-16, -4.647091401871169758, -3.272172305156503480 ) ) ;
#13586 = DIRECTION ( 'NONE',  ( 1.000000000000000000, 1.276920294826118092E-16, -0.000000000000000000 ) ) ;
#13587 = VECTOR ( 'NONE', #10780, 1000.000000000000000 ) ;
#13588 = VERTEX_POINT ( 'NONE', #6096 ) ;
#13589 = LINE ( 'NONE', #120, #1410 ) ;
#13590 = ORIENTED_EDGE ( 'NONE', *, *, #12872, .T. ) ;
#13591 = CARTESIAN_POINT ( 'NONE',  ( 47.05443476855437268, 62.09002498982675888, 25.00000000000000000 ) ) ;
#13592 = VECTOR ( 'NONE', #10166, 1000.000000000000000 ) ;
#13593 = ADVANCED_FACE ( 'NONE', ( #10578, #2833, #11258, #12611, #6786, #564, #8293, #5019, #6183, #1569, #1648, #2756, #5081, #11591, #7882, #12361 ), #5946, .F. ) ;
#13594 = ADVANCED_FACE ( 'NONE', ( #9325 ), #10421, .F. ) ;
#13595 = ORIENTED_EDGE ( 'NONE', *, *, #13970, .T. ) ;
#13596 = CARTESIAN_POINT ( 'NONE',  ( 5.005339752383235918, -4.664709065580361802, 0.07951310411232598296 ) ) ;
#13597 = AXIS2_PLACEMENT_3D ( 'NONE', #14063, #5111, #3014 ) ;
#13598 = ORIENTED_EDGE ( 'NONE', *, *, #11241, .T. ) ;
#13599 = EDGE_LOOP ( 'NONE', ( #8513, #11979, #6475, #6331, #6658, #7408 ) ) ;
#13600 = VECTOR ( 'NONE', #3399, 1000.000000000000000 ) ;
#13601 = EDGE_CURVE ( 'NONE', #10551, #658, #5657, .T. ) ;
#13602 = ORIENTED_EDGE ( 'NONE', *, *, #10840, .T. ) ;
#13603 = DIRECTION ( 'NONE',  ( 0.000000000000000000, 0.000000000000000000, -1.000000000000000000 ) ) ;
#13604 = ORIENTED_EDGE ( 'NONE', *, *, #141, .T. ) ;
#13605 = DIRECTION ( 'NONE',  ( 0.9240638205168504316, 0.3822382184081046796, 0.000000000000000000 ) ) ;
#13606 = CARTESIAN_POINT ( 'NONE',  ( 5.236773790937433226, 1.020504364866074987, -4.356121212116739194 ) ) ;
#13607 = DIRECTION ( 'NONE',  ( 0.000000000000000000, 0.000000000000000000, -1.000000000000000000 ) ) ;
#13608 = CONICAL_SURFACE ( 'NONE', #11017, 2.100000000000000977, 1.029744258676656754 ) ;
#13609 = CARTESIAN_POINT ( 'NONE',  ( 56.99999999999997868, -8.673617379884035472E-16, 25.00000000000000000 ) ) ;
#13610 = MECHANICAL_DESIGN_GEOMETRIC_PRESENTATION_REPRESENTATION (  '', ( #2372 ), #8681 ) ;
#13611 = CIRCLE ( 'NONE', #740, 2.100000000000000977 ) ;
#13612 = VERTEX_POINT ( 'NONE', #7197 ) ;
#13613 = CONTEXT_DEPENDENT_SHAPE_REPRESENTATION ( #11962, #5452 ) ;
#13614 = CARTESIAN_POINT ( 'NONE',  ( 58.68170757442803165, 34.50422595846454499, -28.00000000000000000 ) ) ;
#13615 = CARTESIAN_POINT ( 'NONE',  ( -3.999999999999990674, -1.680125368658683671, -3.016613018637997357 ) ) ;
#13616 = CARTESIAN_POINT ( 'NONE',  ( 39.85300976710104948, 100.8957249956400375, 25.00000000000000000 ) ) ;
#13617 = AXIS2_PLACEMENT_3D ( 'NONE', #5024, #413, #4947 ) ;
#13618 = CIRCLE ( 'NONE', #1449, 2.500000000000002220 ) ;
#13619 = ORIENTED_EDGE ( 'NONE', *, *, #7793, .F. ) ;
#13620 = VECTOR ( 'NONE', #8569, 1000.000000000000000 ) ;
#13621 = VECTOR ( 'NONE', #14305, 1000.000000000000000 ) ;
#13622 = ORIENTED_EDGE ( 'NONE', *, *, #2392, .F. ) ;
#13623 = PLANE ( 'NONE',  #1512 ) ;
#13624 = VERTEX_POINT ( 'NONE', #5683 ) ;
#13625 = ORIENTED_EDGE ( 'NONE', *, *, #9460, .F. ) ;
#13626 = DIRECTION ( 'NONE',  ( 3.916739600140467622E-15, -1.000000000000000000, -0.000000000000000000 ) ) ;
#13627 = CARTESIAN_POINT ( 'NONE',  ( 4.872112557121028864, 0.7881298154076051832, -4.072377784234137543 ) ) ;
#13628 = CARTESIAN_POINT ( 'NONE',  ( -5.236972091263603524, 1.063041182845755772, -4.359263227153169495 ) ) ;
#13629 = DIRECTION ( 'NONE',  ( -0.9701425001453318764, -0.2425356250363329969, 0.000000000000000000 ) ) ;
#13630 = CARTESIAN_POINT ( 'NONE',  ( 36.31750732272606541, 144.5765550933605823, -33.00000000000000000 ) ) ;
#13631 = PRESENTATION_STYLE_ASSIGNMENT (( #10170 ) ) ;
#13632 = CARTESIAN_POINT ( 'NONE',  ( 108.6817075744280601, 189.5765550933606107, 33.00000000000002842 ) ) ;
#13633 = VECTOR ( 'NONE', #12654, 1000.000000000000000 ) ;
#13634 = VECTOR ( 'NONE', #9524, 1000.000000000000000 ) ;
#13635 = ADVANCED_FACE ( 'NONE', ( #7048 ), #5878, .F. ) ;
#13636 = EDGE_CURVE ( 'NONE', #698, #7122, #13469, .T. ) ;
#13637 = VERTEX_POINT ( 'NONE', #1504 ) ;
#13638 = CARTESIAN_POINT ( 'NONE',  ( 71.80728622811317052, -17.99808865627607801, -25.00000000000000000 ) ) ;
#13639 = ORIENTED_EDGE ( 'NONE', *, *, #12141, .F. ) ;
#13640 = ORIENTED_EDGE ( 'NONE', *, *, #2475, .T. ) ;
#13641 = ORIENTED_EDGE ( 'NONE', *, *, #8616, .T. ) ;
#13642 = VECTOR ( 'NONE', #8222, 1000.000000000000000 ) ;
#13643 = DIRECTION ( 'NONE',  ( 1.913084959030911013E-15, -1.000000000000000000, 0.000000000000000000 ) ) ;
#13644 = CARTESIAN_POINT ( 'NONE',  ( 3.973110223767151616, -2.262970274364543210E-11, -3.565797985667430225 ) ) ;
#13645 = EDGE_CURVE ( 'NONE', #12237, #5054, #13811, .T. ) ;
#13646 = VERTEX_POINT ( 'NONE', #2681 ) ;
#13647 = ADVANCED_FACE ( 'NONE', ( #7121 ), #7413, .T. ) ;
#13648 = ORIENTED_EDGE ( 'NONE', *, *, #2311, .F. ) ;
#13649 = FACE_OUTER_BOUND ( 'NONE', #7807, .T. ) ;
#13650 = AXIS2_PLACEMENT_3D ( 'NONE', #8788, #2143, #11062 ) ;
#13651 = DIRECTION ( 'NONE',  ( 0.000000000000000000, 0.000000000000000000, 1.000000000000000000 ) ) ;
#13652 = ORIENTED_EDGE ( 'NONE', *, *, #3970, .T. ) ;
#13653 = DIRECTION ( 'NONE',  ( 1.000000000000000000, 0.000000000000000000, 0.000000000000000000 ) ) ;
#13654 = B_SPLINE_CURVE_WITH_KNOTS ( 'NONE', 3,
 ( #119, #6900, #3351, #2243, #11305 ),
 .UNSPECIFIED., .F., .F.,
 ( 4, 1, 4 ),
 ( 0.000000000000000000, 0.002020725942163686603, 0.004041451884327373206 ),
 .UNSPECIFIED. ) ;
#13655 = ORIENTED_EDGE ( 'NONE', *, *, #8337, .T. ) ;
#13656 = UNCERTAINTY_MEASURE_WITH_UNIT (LENGTH_MEASURE( 1.000000000000000082E-05 ), #13449, 'distance_accuracy_value', 'NONE');
#13657 = DIRECTION ( 'NONE',  ( 0.000000000000000000, 1.000000000000000000, 0.000000000000000000 ) ) ;
#13658 = CARTESIAN_POINT ( 'NONE',  ( 24.99999999999999289, -4.898587196589414604E-15, -25.00000000000000000 ) ) ;
#13659 = VERTEX_POINT ( 'NONE', #2983 ) ;
#13660 = EDGE_CURVE ( 'NONE', #2270, #1103, #9887, .T. ) ;
#13661 = CARTESIAN_POINT ( 'NONE',  ( -2.930059260563458778, -4.081832189068413719, -1.671478349248484320E-14 ) ) ;
#13662 = FACE_BOUND ( 'NONE', #11315, .T. ) ;
#13663 = DIRECTION ( 'NONE',  ( 1.000000000000000000, 0.000000000000000000, 0.000000000000000000 ) ) ;
#13664 = CARTESIAN_POINT ( 'NONE',  ( 108.6817075744280743, -20.42344490663954204, -106.9999999999999858 ) ) ;
#13665 = EDGE_LOOP ( 'NONE', ( #6976, #8659, #4870, #11956 ) ) ;
#13666 = DIRECTION ( 'NONE',  ( 0.000000000000000000, 1.000000000000000000, 0.000000000000000000 ) ) ;
#13667 = ORIENTED_EDGE ( 'NONE', *, *, #7242, .F. ) ;
#13668 = DIRECTION ( 'NONE',  ( 0.000000000000000000, 0.000000000000000000, 1.000000000000000000 ) ) ;
#13669 = CARTESIAN_POINT ( 'NONE',  ( 4.140405595019061913, 2.228337868678513800, -3.386887224136951868 ) ) ;
#13670 = VERTEX_POINT ( 'NONE', #6325 ) ;
#13671 = DIRECTION ( 'NONE',  ( 0.000000000000000000, 0.000000000000000000, -1.000000000000000000 ) ) ;
#13672 = VERTEX_POINT ( 'NONE', #14312 ) ;
#13673 = ORIENTED_EDGE ( 'NONE', *, *, #2264, .T. ) ;
#13674 = ORIENTED_EDGE ( 'NONE', *, *, #1727, .F. ) ;
#13675 = DIRECTION ( 'NONE',  ( 0.000000000000000000, 1.000000000000000000, 0.000000000000000000 ) ) ;
#13676 = DIRECTION ( 'NONE',  ( 0.000000000000000000, 1.000000000000000000, 0.000000000000000000 ) ) ;
#13677 = AXIS2_PLACEMENT_3D ( 'NONE', #10897, #5339, #940 ) ;
#13678 = EDGE_CURVE ( 'NONE', #8390, #12991, #12747, .T. ) ;
#13679 = ORIENTED_EDGE ( 'NONE', *, *, #5896, .T. ) ;
#13680 = CARTESIAN_POINT ( 'NONE',  ( 4.000000000000003553, 2.309401076758511806, -0.5000000000000004441 ) ) ;
#13681 = EDGE_CURVE ( 'NONE', #3463, #11019, #977, .T. ) ;
#13682 = CARTESIAN_POINT ( 'NONE',  ( 5.000000000000001776, -1.088253076326978874, -4.021000279465625660 ) ) ;
#13683 = DIRECTION ( 'NONE',  ( -0.000000000000000000, -0.000000000000000000, -1.000000000000000000 ) ) ;
#13684 = DIRECTION ( 'NONE',  ( -8.673617379882015172E-19, -0.8660254037844380415, 0.5000000000000012212 ) ) ;
#13685 = CARTESIAN_POINT ( 'NONE',  ( -31.44014396567295577, 38.31657438465165200, 8.000000000000007105 ) ) ;
#13686 = B_SPLINE_CURVE_WITH_KNOTS ( 'NONE', 3,
 ( #14121, #8470, #13024, #5099, #10671, #3000, #7431, #13968 ),
 .UNSPECIFIED., .F., .F.,
 ( 4, 2, 2, 4 ),
 ( 2.451332856810592536E-07, 0.001475502392055651462, 0.002213131021440637152, 0.002950759650825622842 ),
 .UNSPECIFIED. ) ;
#13687 = CARTESIAN_POINT ( 'NONE',  ( 59.10586122665984732, -20.42344490663941414, 35.00000000000000000 ) ) ;
#13688 = CARTESIAN_POINT ( 'NONE',  ( 23.40000000000000213, 29.99999999999999645, -34.50000000000000000 ) ) ;
#13689 = CARTESIAN_POINT ( 'NONE',  ( 4.093692494532781723, 2.021783646005765878, -3.501831996793842272 ) ) ;
#13690 = ORIENTED_EDGE ( 'NONE', *, *, #10902, .T. ) ;
#13691 = DIRECTION ( 'NONE',  ( -1.000000000000000000, 0.000000000000000000, 0.000000000000000000 ) ) ;
#13692 = CARTESIAN_POINT ( 'NONE',  ( 31.38313257588138683, 143.6985259526510390, 28.00000000000000000 ) ) ;
#13693 = ADVANCED_FACE ( 'NONE', ( #4001 ), #1872, .T. ) ;
#13694 = CARTESIAN_POINT ( 'NONE',  ( 5.599999999999994316, 0.000000000000000000, 0.000000000000000000 ) ) ;
#13695 = SURFACE_STYLE_FILL_AREA ( #5622 ) ;
#13696 = CARTESIAN_POINT ( 'NONE',  ( -5.922811742559419150E-15, -3.857556137907073524, 1.318516776095761234 ) ) ;
#13697 = EDGE_LOOP ( 'NONE', ( #6025, #2668, #10584, #6314 ) ) ;
#13698 = CARTESIAN_POINT ( 'NONE',  ( 0.000000000000000000, 189.5765550933606107, -117.0000000000000000 ) ) ;
#13699 = CARTESIAN_POINT ( 'NONE',  ( 0.000000000000000000, 25.49999999999996803, -22.25000000000000355 ) ) ;
#13700 = CARTESIAN_POINT ( 'NONE',  ( 40.00000000000000711, 80.00000000000000000, -25.00000000000000000 ) ) ;
#13701 = CARTESIAN_POINT ( 'NONE',  ( 0.000000000000000000, 0.000000000000000000, 2.400000000000013234 ) ) ;
#13702 = ORIENTED_EDGE ( 'NONE', *, *, #1297, .F. ) ;
#13703 = B_SPLINE_CURVE_WITH_KNOTS ( 'NONE', 3,
 ( #14424, #8776, #13254, #83, #3231, #4484, #11119, #11185 ),
 .UNSPECIFIED., .F., .F.,
 ( 4, 2, 2, 4 ),
 ( 0.007260997678543204201, 0.007995810154593245220, 0.008730622630643287974, 0.01020024758274337001 ),
 .UNSPECIFIED. ) ;
#13704 = CIRCLE ( 'NONE', #4134, 5.000000000000018652 ) ;
#13705 = ORIENTED_EDGE ( 'NONE', *, *, #12291, .F. ) ;
#13706 = EDGE_LOOP ( 'NONE', ( #13546, #951, #10396 ) ) ;
#13707 = EDGE_CURVE ( 'NONE', #6374, #7758, #779, .T. ) ;
#13708 = CARTESIAN_POINT ( 'NONE',  ( 5.108705940669676870, -2.340113889543992354, 4.101834868599441464 ) ) ;
#13709 = CARTESIAN_POINT ( 'NONE',  ( 0.000000000000000000, 0.000000000000000000, 0.000000000000000000 ) ) ;
#13710 = ORIENTED_EDGE ( 'NONE', *, *, #12453, .F. ) ;
#13711 = VERTEX_POINT ( 'NONE', #11973 ) ;
#13712 = DIRECTION ( 'NONE',  ( -1.000000000000000000, 0.000000000000000000, 0.000000000000000000 ) ) ;
#13713 = CARTESIAN_POINT ( 'NONE',  ( 5.102759246810640192, 2.353060785250084219, -4.075620833350987127 ) ) ;
#13714 = VERTEX_POINT ( 'NONE', #5444 ) ;
#13715 = EDGE_CURVE ( 'NONE', #3061, #8941, #11346, .T. ) ;
#13716 = DIRECTION ( 'NONE',  ( -1.000000000000000000, 0.000000000000000000, 0.000000000000000000 ) ) ;
#13717 = ORIENTED_EDGE ( 'NONE', *, *, #12804, .F. ) ;
#13718 = ADVANCED_FACE ( 'NONE', ( #9624 ), #10864, .F. ) ;
#13719 = LINE ( 'NONE', #6960, #8894 ) ;
#13720 = DIRECTION ( 'NONE',  ( 0.000000000000000000, 0.000000000000000000, -1.000000000000000000 ) ) ;
#13721 = CARTESIAN_POINT ( 'NONE',  ( 4.071447262713911996, -2.020725942163681399, -3.500000000000010214 ) ) ;
#13722 = DIRECTION ( 'NONE',  ( -2.273843122241288438E-18, -5.551115123125783935E-17, -1.000000000000000000 ) ) ;
#13723 = DIRECTION ( 'NONE',  ( 0.000000000000000000, 0.000000000000000000, 1.000000000000000000 ) ) ;
#13724 = CARTESIAN_POINT ( 'NONE',  ( 0.000000000000000000, 25.49999999999996803, 8.000000000000007105 ) ) ;
#13725 = ORIENTED_EDGE ( 'NONE', *, *, #2770, .F. ) ;
#13726 = CARTESIAN_POINT ( 'NONE',  ( -3.822382184081048351, 49.74063820516850143, 0.000000000000000000 ) ) ;
#13727 = VERTEX_POINT ( 'NONE', #835 ) ;
#13728 = CARTESIAN_POINT ( 'NONE',  ( -5.000000000000000000, 2.886751345948124214, -4.284345921091780696 ) ) ;
#13729 = AXIS2_PLACEMENT_3D ( 'NONE', #4835, #2651, #5701 ) ;
#13730 = DIRECTION ( 'NONE',  ( -1.000000000000000000, 0.000000000000000000, 0.000000000000000000 ) ) ;
#13731 = VERTEX_POINT ( 'NONE', #5299 ) ;
#13732 = CARTESIAN_POINT ( 'NONE',  ( 108.6817075744280174, 69.57655509336049704, 1.592040838891559450E-14 ) ) ;
#13733 = EDGE_CURVE ( 'NONE', #11916, #7552, #14332, .T. ) ;
#13734 = CARTESIAN_POINT ( 'NONE',  ( 4.175813232069169878, -2.061359961916364725, 3.570380186727409200 ) ) ;
#13735 = ORIENTED_EDGE ( 'NONE', *, *, #6968, .F. ) ;
#13736 = CARTESIAN_POINT ( 'NONE',  ( 5.067058822021044406, 4.651083900313779829, 4.104209016975491201E-18 ) ) ;
#13737 = VERTEX_POINT ( 'NONE', #4225 ) ;
#13738 = AXIS2_PLACEMENT_3D ( 'NONE', #12848, #11827, #1947 ) ;
#13739 = EDGE_LOOP ( 'NONE', ( #5275, #7250 ) ) ;
#13740 = DIRECTION ( 'NONE',  ( -1.000000000000000000, 2.551526159633733968E-19, 1.987661601597216239E-18 ) ) ;
#13741 = CARTESIAN_POINT ( 'NONE',  ( -2.018703368236236084, 48.24437551459758566, 7.463024472244906171 ) ) ;
#13742 = ORIENTED_EDGE ( 'NONE', *, *, #2065, .T. ) ;
#13743 = ADVANCED_FACE ( 'NONE', ( #707, #8665, #10927, #901, #13219, #5371, #9914, #9834, #3191, #7619, #12109, #2913, #10999, #7352, #11828, #1801 ), #4091, .F. ) ;
#13744 = CARTESIAN_POINT ( 'NONE',  ( 51.97979101891770171, 52.38859998837343568, 25.00000000000000000 ) ) ;
#13745 = DIRECTION ( 'NONE',  ( 0.000000000000000000, -8.482162385747133845E-47, 1.000000000000000000 ) ) ;
#13746 = PLANE ( 'NONE',  #8619 ) ;
#13747 = FACE_OUTER_BOUND ( 'NONE', #13221, .T. ) ;
#13748 = DIRECTION ( 'NONE',  ( 1.000000000000000000, 0.000000000000000000, 0.000000000000000000 ) ) ;
#13749 = DIRECTION ( 'NONE',  ( 0.2425356250363327748, -0.9701425001453319874, -0.000000000000000000 ) ) ;
#13750 = VECTOR ( 'NONE', #5575, 1000.000000000000114 ) ;
#13751 = CARTESIAN_POINT ( 'NONE',  ( 4.166666666666667851, -3.367876570272840819, -4.118275046351178581 ) ) ;
#13752 = PLANE ( 'NONE',  #9385 ) ;
#13753 = VECTOR ( 'NONE', #14268, 1000.000000000000000 ) ;
#13754 = CARTESIAN_POINT ( 'NONE',  ( 0.000000000000000000, 4.618802153517016507, -3.133295621305376422 ) ) ;
#13755 = ORIENTED_EDGE ( 'NONE', *, *, #10702, .F. ) ;
#13756 = EDGE_CURVE ( 'NONE', #7272, #2270, #3334, .T. ) ;
#13757 = ORIENTED_EDGE ( 'NONE', *, *, #2348, .F. ) ;
#13758 = CARTESIAN_POINT ( 'NONE',  ( -0.5276476219777461729, 4.314164656930889130, -3.020318136128642195 ) ) ;
#13759 = ORIENTED_EDGE ( 'NONE', *, *, #5681, .T. ) ;
#13760 = CIRCLE ( 'NONE', #11396, 2.500000000000002220 ) ;
#13761 = ORIENTED_EDGE ( 'NONE', *, *, #11689, .F. ) ;
#13762 = VECTOR ( 'NONE', #6336, 1000.000000000000000 ) ;
#13763 = DIRECTION ( 'NONE',  ( 0.000000000000000000, 0.000000000000000000, -1.000000000000000000 ) ) ;
#13764 = LINE ( 'NONE', #8174, #12221 ) ;
#13765 = LINE ( 'NONE', #3734, #1619 ) ;
#13766 = AXIS2_PLACEMENT_3D ( 'NONE', #1339, #5716, #3488 ) ;
#13767 = DIRECTION ( 'NONE',  ( -1.000000000000000000, -0.000000000000000000, -0.000000000000000000 ) ) ;
#13768 = DIRECTION ( 'NONE',  ( 8.673617379882821173E-19, 0.5000000000000005551, -0.8660254037844383745 ) ) ;
#13769 = CARTESIAN_POINT ( 'NONE',  ( 2.602085213965210642E-15, 5.773502691896270633, 0.000000000000000000 ) ) ;
#13770 = DIRECTION ( 'NONE',  ( 8.658726361542619729E-32, -5.046468293750711996E-16, 1.000000000000000000 ) ) ;
#13771 = CARTESIAN_POINT ( 'NONE',  ( 22.00000000000000711, 17.00000000000000000, -25.00000000000000000 ) ) ;
#13772 = EDGE_CURVE ( 'NONE', #4104, #6300, #4513, .T. ) ;
#13773 = MECHANICAL_DESIGN_GEOMETRIC_PRESENTATION_REPRESENTATION (  '', ( #10015 ), #3720 ) ;
#13774 = ADVANCED_FACE ( 'NONE', ( #13503 ), #2296, .T. ) ;
#13775 = CARTESIAN_POINT ( 'NONE',  ( -5.551115123125782702E-14, -3.464101615137743728, -2.000000000000015543 ) ) ;
#13776 = ORIENTED_EDGE ( 'NONE', *, *, #7205, .T. ) ;
#13777 = EDGE_LOOP ( 'NONE', ( #459, #6449, #1402 ) ) ;
#13778 = EDGE_CURVE ( 'NONE', #6205, #8584, #9168, .T. ) ;
#13779 = CARTESIAN_POINT ( 'NONE',  ( 3.822382184081048351, 49.74063820516850143, 8.000000000000007105 ) ) ;
#13780 = CARTESIAN_POINT ( 'NONE',  ( -3.822382184081048351, 49.74063820516850143, 8.000000000000007105 ) ) ;
#13781 =( NAMED_UNIT ( * ) PLANE_ANGLE_UNIT ( ) SI_UNIT ( $, .RADIAN. ) );
#13782 = CIRCLE ( 'NONE', #5809, 2.445500000000002672 ) ;
#13783 = VERTEX_POINT ( 'NONE', #7845 ) ;
#13784 = CARTESIAN_POINT ( 'NONE',  ( -4.211140560182201398, -2.431303136016548017, -3.445885042887453231 ) ) ;
#13785 = EDGE_CURVE ( 'NONE', #11019, #6031, #11216, .T. ) ;
#13786 = CARTESIAN_POINT ( 'NONE',  ( 5.103531824934171013, 2.354098498486459246, -4.077418205400141105 ) ) ;
#13787 = ORIENTED_EDGE ( 'NONE', *, *, #13091, .T. ) ;
#13788 = DIRECTION ( 'NONE',  ( 0.000000000000000000, 0.000000000000000000, -1.000000000000000000 ) ) ;
#13789 = ORIENTED_EDGE ( 'NONE', *, *, #14144, .T. ) ;
#13790 = VECTOR ( 'NONE', #4894, 1000.000000000000000 ) ;
#13791 = EDGE_LOOP ( 'NONE', ( #10126, #899, #8982, #829, #4443, #10790 ) ) ;
#13792 = UNCERTAINTY_MEASURE_WITH_UNIT (LENGTH_MEASURE( 1.000000000000000082E-05 ), #10331, 'distance_accuracy_value', 'NONE');
#13793 = CARTESIAN_POINT ( 'NONE',  ( 24.99999999999999289, -4.898587196589414604E-15, 25.00000000000000000 ) ) ;
#13794 = CARTESIAN_POINT ( 'NONE',  ( 4.093692494532780835, 2.021783646005765878, 3.501831996793842716 ) ) ;
#13795 = CARTESIAN_POINT ( 'NONE',  ( 4.170895651974821483, -2.054890354522748375, -3.559174498016296706 ) ) ;
#13796 = LINE ( 'NONE', #547, #606 ) ;
#13797 = FILL_AREA_STYLE ('',( #9315 ) ) ;
#13798 = CARTESIAN_POINT ( 'NONE',  ( 30.15499999999998693, 0.000000000000000000, 0.000000000000000000 ) ) ;
#13799 = ADVANCED_FACE ( 'NONE', ( #2232 ), #3477, .F. ) ;
#13800 = CARTESIAN_POINT ( 'NONE',  ( 60.00000000000000000, -6.123233995736768255E-16, 23.00000000000000000 ) ) ;
#13801 = ORIENTED_EDGE ( 'NONE', *, *, #13933, .T. ) ;
#13802 = ADVANCED_BREP_SHAPE_REPRESENTATION ( '', ( #11581, #11025 ), #11250 ) ;
#13803 = CARTESIAN_POINT ( 'NONE',  ( 71.80728622811317052, -17.99808865627607801, 25.00000000000000000 ) ) ;
#13804 = VECTOR ( 'NONE', #9935, 1000.000000000000000 ) ;
#13805 = PLANE ( 'NONE',  #9528 ) ;
#13806 = CYLINDRICAL_SURFACE ( 'NONE', #86, 2.499999999999999112 ) ;
#13807 = EDGE_CURVE ( 'NONE', #14315, #11970, #4369, .T. ) ;
#13808 = ORIENTED_EDGE ( 'NONE', *, *, #12278, .T. ) ;
#13809 = CARTESIAN_POINT ( 'NONE',  ( 4.962664318265050056, -4.324618243610393264, -0.6590959511430992679 ) ) ;
#13810 = EDGE_CURVE ( 'NONE', #630, #7983, #2812, .T. ) ;
#13811 = LINE ( 'NONE', #3779, #13642 ) ;
#13812 = ORIENTED_EDGE ( 'NONE', *, *, #11035, .T. ) ;
#13813 = CARTESIAN_POINT ( 'NONE',  ( 5.098157279264013297, 4.694029454718616989, 9.324225811086985581E-14 ) ) ;
#13814 = ORIENTED_EDGE ( 'NONE', *, *, #7993, .F. ) ;
#13815 = VECTOR ( 'NONE', #4544, 1000.000000000000000 ) ;
#13816 = VERTEX_POINT ( 'NONE', #1269 ) ;
#13817 = AXIS2_PLACEMENT_3D ( 'NONE', #1492, #7994, #8132 ) ;
#13818 = CARTESIAN_POINT ( 'NONE',  ( 76.68170757442801744, 29.57655509336063204, 33.00000000000000000 ) ) ;
#13819 = DIRECTION ( 'NONE',  ( -1.000000000000000000, 0.000000000000000000, 0.000000000000000000 ) ) ;
#13820 = AXIS2_PLACEMENT_3D ( 'NONE', #6512, #4431, #14037 ) ;
#13821 = DIRECTION ( 'NONE',  ( 0.000000000000000000, 0.000000000000000000, -1.000000000000000000 ) ) ;
#13822 = FACE_OUTER_BOUND ( 'NONE', #6677, .T. ) ;
#13823 = ADVANCED_FACE ( 'NONE', ( #13286 ), #8948, .T. ) ;
#13824 = ADVANCED_FACE ( 'NONE', ( #12179 ), #6839, .T. ) ;
#13825 = DIRECTION ( 'NONE',  ( 1.000000000000000000, 1.224646799147353454E-16, -0.000000000000000000 ) ) ;
#13826 = DIRECTION ( 'NONE',  ( 0.000000000000000000, 0.000000000000000000, -1.000000000000000000 ) ) ;
#13827 = CARTESIAN_POINT ( 'NONE',  ( 32.57694101601105530, 130.0000000000000000, 25.00000000000000000 ) ) ;
#13828 = CARTESIAN_POINT ( 'NONE',  ( -1.752700365193367750E-15, -5.773502691896304384, -4.284345921091780696 ) ) ;
#13829 = VECTOR ( 'NONE', #12780, 1000.000000000000000 ) ;
#13830 = DIRECTION ( 'NONE',  ( 0.000000000000000000, 0.000000000000000000, -1.000000000000000000 ) ) ;
#13831 = PRESENTATION_LAYER_ASSIGNMENT (  '', '', ( #12171 ) ) ;
#13832 = CARTESIAN_POINT ( 'NONE',  ( 20.00000000000000000, 60.00000000000000711, 25.00000000000000000 ) ) ;
#13833 = ORIENTED_EDGE ( 'NONE', *, *, #9421, .T. ) ;
#13834 = CARTESIAN_POINT ( 'NONE',  ( -3.065261730689029740, 7.410293710401353984, 8.000000000000007105 ) ) ;
#13835 = EDGE_LOOP ( 'NONE', ( #7804, #12686, #3480, #11393 ) ) ;
#13836 = ORIENTED_EDGE ( 'NONE', *, *, #5830, .T. ) ;
#13837 = PLANE ( 'NONE',  #6058 ) ;
#13838 = CIRCLE ( 'NONE', #5411, 2.500000000000002220 ) ;
#13839 = CARTESIAN_POINT ( 'NONE',  ( 31.44014396567294867, 38.31657438465161647, 8.000000000000007105 ) ) ;
#13840 = CARTESIAN_POINT ( 'NONE',  ( 20.00000000000000000, 78.00000000000000000, 25.00000000000000000 ) ) ;
#13841 = DIRECTION ( 'NONE',  ( 0.000000000000000000, 0.000000000000000000, -1.000000000000000000 ) ) ;
#13842 = EDGE_CURVE ( 'NONE', #2603, #8545, #1125, .T. ) ;
#13843 = DIRECTION ( 'NONE',  ( -0.000000000000000000, -1.000000000000000000, -0.000000000000000000 ) ) ;
#13844 = CARTESIAN_POINT ( 'NONE',  ( 0.000000000000000000, 0.8660254037844428154, -1.500000000000001332 ) ) ;
#13845 = DIRECTION ( 'NONE',  ( 1.000000000000000000, 0.000000000000000000, 0.000000000000000000 ) ) ;
#13846 = DIRECTION ( 'NONE',  ( -1.000000000000000000, -1.224646799147353454E-16, 0.000000000000000000 ) ) ;
#13847 = FACE_OUTER_BOUND ( 'NONE', #14264, .T. ) ;
#13848 = AXIS2_PLACEMENT_3D ( 'NONE', #5739, #12711, #11391 ) ;
#13849 = AXIS2_PLACEMENT_3D ( 'NONE', #12802, #10536, #733 ) ;
#13850 = DIRECTION ( 'NONE',  ( 0.000000000000000000, 0.000000000000000000, 1.000000000000000000 ) ) ;
#13851 = VERTEX_POINT ( 'NONE', #2370 ) ;
#13852 = ORIENTED_EDGE ( 'NONE', *, *, #8784, .T. ) ;
#13853 = PLANE ( 'NONE',  #5046 ) ;
#13854 = DIRECTION ( 'NONE',  ( 0.000000000000000000, 0.000000000000000000, -1.000000000000000000 ) ) ;
#13855 = VECTOR ( 'NONE', #1644, 1000.000000000000000 ) ;
#13856 = EDGE_CURVE ( 'NONE', #1484, #3708, #8934, .T. ) ;
#13857 = AXIS2_PLACEMENT_3D ( 'NONE', #13426, #12086, #11130 ) ;
#13858 = PRODUCT_DEFINITION ( 'UNKNOWN', '', #5678, #5834 ) ;
#13859 = EDGE_CURVE ( 'NONE', #7983, #7481, #7501, .T. ) ;
#13860 = FILL_AREA_STYLE_COLOUR ( '', #2153 ) ;
#13861 = ORIENTED_EDGE ( 'NONE', *, *, #5769, .F. ) ;
#13862 = VERTEX_POINT ( 'NONE', #9981 ) ;
#13863 = CARTESIAN_POINT ( 'NONE',  ( 0.8441225671340620851, -5.568793373800590807, -4.476900509771624570 ) ) ;
#13864 = CARTESIAN_POINT ( 'NONE',  ( -140.0000000000003411, 189.5765550933606107, 47.99999999999998579 ) ) ;
#13865 = VERTEX_POINT ( 'NONE', #4582 ) ;
#13866 = MECHANICAL_DESIGN_GEOMETRIC_PRESENTATION_REPRESENTATION (  '', ( #12930 ), #11281 ) ;
#13867 = LINE ( 'NONE', #7249, #12670 ) ;
#13868 = VERTEX_POINT ( 'NONE', #170 ) ;
#13869 = PRODUCT_DEFINITION_SHAPE ( 'NONE', 'NONE',  #8013 ) ;
#13870 = CARTESIAN_POINT ( 'NONE',  ( -0.6937372685066646172, 4.453844082567730567, -3.310536846335873751 ) ) ;
#13871 = LINE ( 'NONE', #8057, #11290 ) ;
#13872 = DIRECTION ( 'NONE',  ( -0.7071067811865513475, 1.601178185494237639E-17, 0.7071067811865435759 ) ) ;
#13873 = CARTESIAN_POINT ( 'NONE',  ( 56.99999999999997868, -8.673617379884035472E-16, -23.00000000000000000 ) ) ;
#13874 = CARTESIAN_POINT ( 'NONE',  ( 37.35300976710104948, 100.8957249956400375, -25.00000000000000000 ) ) ;
#13875 = AXIS2_PLACEMENT_3D ( 'NONE', #468, #8208, #13720 ) ;
#13876 = DIRECTION ( 'NONE',  ( -0.000000000000000000, -0.000000000000000000, -1.000000000000000000 ) ) ;
#13877 = ORIENTED_EDGE ( 'NONE', *, *, #834, .F. ) ;
#13878 = ORIENTED_EDGE ( 'NONE', *, *, #7242, .T. ) ;
#13879 = CARTESIAN_POINT ( 'NONE',  ( 0.000000000000000000, 0.000000000000000000, -25.00000000000000000 ) ) ;
#13880 = CARTESIAN_POINT ( 'NONE',  ( 0.000000000000000000, 0.000000000000000000, -4.674599999999973221 ) ) ;
#13881 = AXIS2_PLACEMENT_3D ( 'NONE', #10208, #2318, #8009 ) ;
#13882 = EDGE_LOOP ( 'NONE', ( #11412, #403 ) ) ;
#13883 = CARTESIAN_POINT ( 'NONE',  ( 4.988724804725896966, -2.309401076758484272, 4.000000000000003553 ) ) ;
#13884 = CARTESIAN_POINT ( 'NONE',  ( 5.005339752383242136, 4.664709065580363578, -0.07951310411231406194 ) ) ;
#13885 = VERTEX_POINT ( 'NONE', #3340 ) ;
#13886 = PRESENTATION_STYLE_ASSIGNMENT (( #3275 ) ) ;
#13887 = DIRECTION ( 'NONE',  ( 1.000000000000000000, 0.000000000000000000, 0.000000000000000000 ) ) ;
#13888 = EDGE_LOOP ( 'NONE', ( #10581, #5774, #9121, #12862, #7141 ) ) ;
#13889 = EDGE_LOOP ( 'NONE', ( #3785, #4188, #8143, #5071 ) ) ;
#13890 = CARTESIAN_POINT ( 'NONE',  ( 8.000000000000000000, 25.49999999999996803, 8.000000000000007105 ) ) ;
#13891 = CARTESIAN_POINT ( 'NONE',  ( 37.42765351673772045, 110.5971499970933536, 25.00000000000000000 ) ) ;
#13892 = DIRECTION ( 'NONE',  ( 1.000000000000000000, 0.000000000000000000, 0.000000000000000000 ) ) ;
#13893 = AXIS2_PLACEMENT_3D ( 'NONE', #14178, #1951, #6399 ) ;
#13894 = ADVANCED_FACE ( 'NONE', ( #4641 ), #7781, .T. ) ;
#13895 = DIRECTION ( 'NONE',  ( 0.000000000000000000, 8.482162385747133845E-47, -1.000000000000000000 ) ) ;
#13896 = LINE ( 'NONE', #12777, #7211 ) ;
#13897 = FACE_BOUND ( 'NONE', #1422, .T. ) ;
#13898 = CONTEXT_DEPENDENT_SHAPE_REPRESENTATION ( #7264, #4313 ) ;
#13899 = CARTESIAN_POINT ( 'NONE',  ( 108.6817075744280459, 189.5765550933606107, -106.9999999999999858 ) ) ;
#13900 = CARTESIAN_POINT ( 'NONE',  ( -3.999999999999990674, -2.472261030551099914, -3.387027369136278665 ) ) ;
#13901 = CARTESIAN_POINT ( 'NONE',  ( 92.68170757442806007, 124.5765550933605965, 25.00000000000000000 ) ) ;
#13902 = EDGE_CURVE ( 'NONE', #7846, #10355, #11729, .T. ) ;
#13903 = LINE ( 'NONE', #13486, #11886 ) ;
#13904 = EDGE_CURVE ( 'NONE', #13229, #8393, #3757, .T. ) ;
#13905 = ORIENTED_EDGE ( 'NONE', *, *, #1612, .F. ) ;
#13906 = DIRECTION ( 'NONE',  ( -0.000000000000000000, 1.000000000000000000, -0.000000000000000000 ) ) ;
#13907 = VERTEX_POINT ( 'NONE', #5000 ) ;
#13908 = ORIENTED_EDGE ( 'NONE', *, *, #6368, .T. ) ;
#13909 = CARTESIAN_POINT ( 'NONE',  ( 92.68170757442806007, 124.5765550933605965, -25.00000000000000000 ) ) ;
#13910 = EDGE_CURVE ( 'NONE', #7536, #13002, #13173, .T. ) ;
#13911 = DIRECTION ( 'NONE',  ( 1.000000000000000000, 0.000000000000000000, 0.000000000000000000 ) ) ;
#13912 = FACE_OUTER_BOUND ( 'NONE', #9270, .T. ) ;
#13913 = CARTESIAN_POINT ( 'NONE',  ( 20.00000000000000000, 60.00000000000000711, 25.00000000000000000 ) ) ;
#13914 = CARTESIAN_POINT ( 'NONE',  ( 5.024612689793206854, -2.312654742478277736, -4.005635514337468450 ) ) ;
#13915 = EDGE_LOOP ( 'NONE', ( #9861, #4703, #6365, #11440 ) ) ;
#13916 = FACE_OUTER_BOUND ( 'NONE', #8897, .T. ) ;
#13917 = DIRECTION ( 'NONE',  ( 0.9237280213470682178, 0.3830490080632377725, 0.000000000000000000 ) ) ;
#13918 = CLOSED_SHELL ( 'NONE', ( #5172, #5082, #10161, #12485, #5768, #13647, #14348, #2253, #5993, #14263, #5429, #11933, #5500, #2691, #8475, #12762, #4488, #11342, #3541 ) ) ;
#13919 = PLANE ( 'NONE',  #14081 ) ;
#13920 = DIRECTION ( 'NONE',  ( 0.000000000000000000, -8.482162385747133845E-47, 1.000000000000000000 ) ) ;
#13921 = CARTESIAN_POINT ( 'NONE',  ( 1.560000000000005826, 0.000000000000000000, 0.000000000000000000 ) ) ;
#13922 = EDGE_CURVE ( 'NONE', #2748, #12258, #6604, .T. ) ;
#13923 = EDGE_LOOP ( 'NONE', ( #3028, #1703, #8492, #474, #8527, #14028 ) ) ;
#13924 = ORIENTED_EDGE ( 'NONE', *, *, #13541, .T. ) ;
#13925 = PLANE ( 'NONE',  #7533 ) ;
#13926 = CARTESIAN_POINT ( 'NONE',  ( 3.973110223768752114, 0.6864646529411640996, 3.565797985667471970 ) ) ;
#13927 = ORIENTED_EDGE ( 'NONE', *, *, #12453, .T. ) ;
#13928 = CARTESIAN_POINT ( 'NONE',  ( 6.799999999999972289, -2.309401076758498039, -4.000000000000003553 ) ) ;
#13929 = CARTESIAN_POINT ( 'NONE',  ( -4.296971609537496128, -3.292644976429660808, -4.396693167836204452 ) ) ;
#13930 = ORIENTED_EDGE ( 'NONE', *, *, #2914, .F. ) ;
#13931 = EDGE_CURVE ( 'NONE', #7235, #3193, #2184, .T. ) ;
#13932 = FACE_BOUND ( 'NONE', #6766, .T. ) ;
#13933 = EDGE_CURVE ( 'NONE', #5517, #14018, #13867, .T. ) ;
#13934 = LINE ( 'NONE', #8350, #13587 ) ;
#13935 = CARTESIAN_POINT ( 'NONE',  ( 108.6817075744280316, 69.57655509336046862, -3.299999999999976730 ) ) ;
#13936 = CARTESIAN_POINT ( 'NONE',  ( 51.90514726928103073, 42.68717498692012668, -25.00000000000000000 ) ) ;
#13937 = EDGE_LOOP ( 'NONE', ( #2951, #11975, #1502, #10359 ) ) ;
#13938 = CARTESIAN_POINT ( 'NONE',  ( 4.124214193018064911, 4.056676826581889550, -6.846764070645731666E-15 ) ) ;
#13939 = DIRECTION ( 'NONE',  ( 0.000000000000000000, 0.000000000000000000, -1.000000000000000000 ) ) ;
#13940 = FILL_AREA_STYLE ('',( #11815 ) ) ;
#13941 = ORIENTED_EDGE ( 'NONE', *, *, #13383, .F. ) ;
#13942 = FACE_OUTER_BOUND ( 'NONE', #13923, .T. ) ;
#13943 = DIRECTION ( 'NONE',  ( -0.000000000000000000, -0.000000000000000000, -1.000000000000000000 ) ) ;
#13944 = EDGE_LOOP ( 'NONE', ( #9199, #9614 ) ) ;
#13945 = ORIENTED_EDGE ( 'NONE', *, *, #3843, .T. ) ;
#13946 = CARTESIAN_POINT ( 'NONE',  ( 2.068360682592138122, 4.579334095020464623, -0.01465562841808510514 ) ) ;
#13947 = DIRECTION ( 'NONE',  ( -1.000000000000000000, -1.665334536937734071E-16, 0.000000000000000000 ) ) ;
#13948 = ORIENTED_EDGE ( 'NONE', *, *, #886, .T. ) ;
#13949 = DIRECTION ( 'NONE',  ( 1.446433017903778039E-17, 0.5000000000000012212, -0.8660254037844380415 ) ) ;
#13950 = EDGE_CURVE ( 'NONE', #11237, #14260, #8735, .T. ) ;
#13951 = CARTESIAN_POINT ( 'NONE',  ( 0.000000000000000000, 25.49999999999996803, 8.000000000000007105 ) ) ;
#13952 = ADVANCED_FACE ( 'NONE', ( #13932, #11501, #9308 ), #12829, .F. ) ;
#13953 = PLANE ( 'NONE',  #3767 ) ;
#13954 = VERTEX_POINT ( 'NONE', #2660 ) ;
#13955 = EDGE_LOOP ( 'NONE', ( #11586, #320, #10229, #10045 ) ) ;
#13956 = LINE ( 'NONE', #2839, #4770 ) ;
#13957 = DIRECTION ( 'NONE',  ( 1.000000000000000000, 1.665334536937734071E-16, 0.000000000000000000 ) ) ;
#13958 = ORIENTED_EDGE ( 'NONE', *, *, #13127, .F. ) ;
#13959 = CARTESIAN_POINT ( 'NONE',  ( 5.102759246810695259, -2.353060785250042475, 4.075620833351015548 ) ) ;
#13960 = DIRECTION ( 'NONE',  ( 0.000000000000000000, 0.000000000000000000, -1.000000000000000000 ) ) ;
#13961 =( LENGTH_UNIT ( ) NAMED_UNIT ( * ) SI_UNIT ( .MILLI., .METRE. ) );
#13962 = CARTESIAN_POINT ( 'NONE',  ( 4.050480423730761004, -1.376911654797407403, 3.567926555162034941 ) ) ;
#13963 = CARTESIAN_POINT ( 'NONE',  ( 0.000000000000000000, 40.49999999999999289, 8.000000000000007105 ) ) ;
#13964 = DIRECTION ( 'NONE',  ( 0.000000000000000000, 0.000000000000000000, -1.000000000000000000 ) ) ;
#13965 = CARTESIAN_POINT ( 'NONE',  ( 20.00000000000000000, 80.00000000000000000, -25.00000000000000000 ) ) ;
#13966 = DIRECTION ( 'NONE',  ( -1.000000000000000000, 1.892425610156516875E-16, 0.000000000000000000 ) ) ;
#13967 = AXIS2_PLACEMENT_3D ( 'NONE', #1412, #13723, #3850 ) ;
#13968 = CARTESIAN_POINT ( 'NONE',  ( 2.500000000000011546, -4.330127018922186544, 0.000000000000000000 ) ) ;
#13969 = CONICAL_SURFACE ( 'NONE', #865, 5.000000000000000888, 0.9110539511682884672 ) ;
#13970 = EDGE_CURVE ( 'NONE', #3697, #3920, #1943, .T. ) ;
#13971 = AXIS2_PLACEMENT_3D ( 'NONE', #64, #7806, #6701 ) ;
#13972 = EDGE_CURVE ( 'NONE', #12327, #2267, #9426, .T. ) ;
#13973 = ORIENTED_EDGE ( 'NONE', *, *, #4383, .T. ) ;
#13974 = DIRECTION ( 'NONE',  ( 0.000000000000000000, 0.000000000000000000, 1.000000000000000000 ) ) ;
#13975 = ADVANCED_FACE ( 'NONE', ( #2505 ), #12592, .T. ) ;
#13976 = ORIENTED_EDGE ( 'NONE', *, *, #10174, .T. ) ;
#13977 = DIRECTION ( 'NONE',  ( 1.000000000000000000, 0.000000000000000000, 0.000000000000000000 ) ) ;
#13978 = CARTESIAN_POINT ( 'NONE',  ( -1.828356344711641102, -3.563200125723192446, -1.069379095908553863E-14 ) ) ;
#13979 = DIRECTION ( 'NONE',  ( 0.000000000000000000, 0.000000000000000000, 1.000000000000000000 ) ) ;
#13980 = VECTOR ( 'NONE', #11664, 1000.000000000000000 ) ;
#13981 = CARTESIAN_POINT ( 'NONE',  ( 129.3408537872138595, 199.5765550933606107, -75.00000000000001421 ) ) ;
#13982 = CARTESIAN_POINT ( 'NONE',  ( 32.42765351673771335, 110.5971499970933536, -25.00000000000000000 ) ) ;
#13983 = CIRCLE ( 'NONE', #3930, 4.750000000000000000 ) ;
#13984 = CARTESIAN_POINT ( 'NONE',  ( 3.822382184081044798, 10.25936179483148969, 0.000000000000000000 ) ) ;
#13985 = DIRECTION ( 'NONE',  ( 0.000000000000000000, 0.000000000000000000, 1.000000000000000000 ) ) ;
#13987 = B_SPLINE_CURVE_WITH_KNOTS ( 'NONE', 3,
 ( #13728, #1345, #7043, #1498, #6844 ),
 .UNSPECIFIED., .F., .F.,
 ( 4, 1, 4 ),
 ( 0.000000000000000000, 0.002886751345948135056, 0.005773502691896270113 ),
 .UNSPECIFIED. ) ;
#13986 = CYLINDRICAL_SURFACE ( 'NONE', #4728, 3.000000000000000888 ) ;
#13988 = EDGE_CURVE ( 'NONE', #1123, #1772, #6957, .T. ) ;
#13989 = DIRECTION ( 'NONE',  ( -0.2425356250363328581, 0.9701425001453318764, 0.000000000000000000 ) ) ;
#13990 = PRODUCT_DEFINITION_SHAPE ( 'NONE', 'NONE',  #14471 ) ;
#13991 = ORIENTED_EDGE ( 'NONE', *, *, #7422, .F. ) ;
#13992 = CARTESIAN_POINT ( 'NONE',  ( 3.500188911486806997, 4.028306647601582746, -4.385926550512752264 ) ) ;
#13993 = EDGE_CURVE ( 'NONE', #4098, #3285, #6071, .T. ) ;
#13994 = ORIENTED_EDGE ( 'NONE', *, *, #4200, .F. ) ;
#13995 = EDGE_CURVE ( 'NONE', #3669, #9772, #12746, .T. ) ;
#13996 = AXIS2_PLACEMENT_3D ( 'NONE', #3035, #7537, #7457 ) ;
#13997 = CIRCLE ( 'NONE', #10463, 2.500000000000002220 ) ;
#13998 = ORIENTED_EDGE ( 'NONE', *, *, #7378, .T. ) ;
#13999 = ORIENTED_EDGE ( 'NONE', *, *, #13529, .T. ) ;
#14000 = AXIS2_PLACEMENT_3D ( 'NONE', #13874, #12757, #1638 ) ;
#14001 = EDGE_CURVE ( 'NONE', #3393, #4966, #9232, .T. ) ;
#14002 = EDGE_LOOP ( 'NONE', ( #3057, #6683 ) ) ;
#14003 = CARTESIAN_POINT ( 'NONE',  ( 0.000000000000000000, 0.000000000000000000, 0.000000000000000000 ) ) ;
#14004 = CARTESIAN_POINT ( 'NONE',  ( 0.000000000000000000, 25.49999999999996803, 8.000000000000007105 ) ) ;
#14005 = ADVANCED_FACE ( 'NONE', ( #5929 ), #6848, .T. ) ;
#14006 = STYLED_ITEM ( 'NONE', ( #3305 ), #6910 ) ;
#14007 = ORIENTED_EDGE ( 'NONE', *, *, #3267, .F. ) ;
#14008 = VERTEX_POINT ( 'NONE', #10406 ) ;
#14009 = CARTESIAN_POINT ( 'NONE',  ( 4.000000000000003553, -2.309401076758511806, -4.699999999999981526 ) ) ;
#14010 = PLANE ( 'NONE',  #3103 ) ;
#14011 = ORIENTED_EDGE ( 'NONE', *, *, #10303, .T. ) ;
#14012 = DIRECTION ( 'NONE',  ( 0.000000000000000000, 0.000000000000000000, 1.000000000000000000 ) ) ;
#14013 = VERTEX_POINT ( 'NONE', #10482 ) ;
#14014 = VECTOR ( 'NONE', #12480, 999.9999999999998863 ) ;
#14015 = DIRECTION ( 'NONE',  ( -0.8660254037844372643, -0.5000000000000023315, -2.348866325434636703E-33 ) ) ;
#14016 = LINE ( 'NONE', #8351, #9983 ) ;
#14017 = CARTESIAN_POINT ( 'NONE',  ( -3.000000000000000000, -1.322063213371142838E-16, 1.599999999999990319 ) ) ;
#14018 = VERTEX_POINT ( 'NONE', #9458 ) ;
#14019 = LINE ( 'NONE', #10712, #7713 ) ;
#14020 = CARTESIAN_POINT ( 'NONE',  ( 2.426025403784448642, 0.000000000000000000, 0.000000000000000000 ) ) ;
#14021 = AXIS2_PLACEMENT_3D ( 'NONE', #3214, #7646, #858 ) ;
#14022 = ORIENTED_EDGE ( 'NONE', *, *, #5871, .T. ) ;
#14023 = CYLINDRICAL_SURFACE ( 'NONE', #2038, 5.499999999999984013 ) ;
#14024 =( REPRESENTATION_RELATIONSHIP ('NONE','NONE', #10295, #8802 ) REPRESENTATION_RELATIONSHIP_WITH_TRANSFORMATION ( #11104 )SHAPE_REPRESENTATION_RELATIONSHIP( ) );
#14025 = ADVANCED_FACE ( 'NONE', ( #1927 ), #2197, .T. ) ;
#14026 = FACE_OUTER_BOUND ( 'NONE', #13387, .T. ) ;
#14027 = EDGE_LOOP ( 'NONE', ( #10381, #9293, #7865, #8804 ) ) ;
#14028 = ORIENTED_EDGE ( 'NONE', *, *, #6989, .F. ) ;
#14029 = DIRECTION ( 'NONE',  ( -1.000000000000000000, 2.551526159633733968E-19, 1.987661601597216239E-18 ) ) ;
#14030 = DIRECTION ( 'NONE',  ( -1.734723475976770694E-18, 4.440892098500620738E-16, 1.000000000000000000 ) ) ;
#14031 = AXIS2_PLACEMENT_3D ( 'NONE', #13530, #8831, #8901 ) ;
#14032 = ORIENTED_EDGE ( 'NONE', *, *, #14047, .F. ) ;
#14033 = DIRECTION ( 'NONE',  ( -2.133709875451472726E-16, 1.000000000000000000, 0.000000000000000000 ) ) ;
#14034 = CARTESIAN_POINT ( 'NONE',  ( 4.870920456765266415, 3.923644220354623791, 1.348744467187277474 ) ) ;
#14035 = ORIENTED_EDGE ( 'NONE', *, *, #5923, .F. ) ;
#14036 = VECTOR ( 'NONE', #11099, 1000.000000000000000 ) ;
#14037 = DIRECTION ( 'NONE',  ( 1.734723475976770694E-18, -4.440892098500621231E-16, -1.000000000000000000 ) ) ;
#14038 = EDGE_LOOP ( 'NONE', ( #4833, #13247, #657 ) ) ;
#14039 = ORIENTED_EDGE ( 'NONE', *, *, #1535, .T. ) ;
#14040 = CARTESIAN_POINT ( 'NONE',  ( 20.00000000000000000, -5.510910596163090344E-15, -25.00000000000000000 ) ) ;
#14041 = CARTESIAN_POINT ( 'NONE',  ( -3.790690275325682812, 47.54583148236282142, 2.696316195168957819 ) ) ;
#14042 = VERTEX_POINT ( 'NONE', #14153 ) ;
#14043 = CARTESIAN_POINT ( 'NONE',  ( 5.084394237956035845, -2.335963250529142332, 4.046007034530258117 ) ) ;
#14044 = CIRCLE ( 'NONE', #14273, 2.500000000000000444 ) ;
#14045 = CARTESIAN_POINT ( 'NONE',  ( -4.166666666666669627, -3.367876570272843928, -4.118275046351176805 ) ) ;
#14046 = DIRECTION ( 'NONE',  ( 1.000000000000000000, 1.723842398015259277E-15, -0.000000000000000000 ) ) ;
#14047 = EDGE_CURVE ( 'NONE', #1073, #5455, #12908, .T. ) ;
#14048 = CARTESIAN_POINT ( 'NONE',  ( 3.973110223765541793, -0.6902454861566503785, 3.565797985667388481 ) ) ;
#14049 = ORIENTED_EDGE ( 'NONE', *, *, #283, .T. ) ;
#14050 = EDGE_CURVE ( 'NONE', #1181, #8562, #5137, .T. ) ;
#14051 = DIRECTION ( 'NONE',  ( 0.000000000000000000, -5.551115123125782702E-17, -1.000000000000000000 ) ) ;
#14052 = CYLINDRICAL_SURFACE ( 'NONE', #7196, 4.599999999999999645 ) ;
#14053 = AXIS2_PLACEMENT_3D ( 'NONE', #5808, #6988, #9113 ) ;
#14054 = VECTOR ( 'NONE', #2899, 1000.000000000000000 ) ;
#14055 = VERTEX_POINT ( 'NONE', #4286 ) ;
#14056 = FACE_OUTER_BOUND ( 'NONE', #8853, .T. ) ;
#14057 = ORIENTED_EDGE ( 'NONE', *, *, #8517, .F. ) ;
#14058 = ORIENTED_EDGE ( 'NONE', *, *, #7869, .F. ) ;
#14059 = DIRECTION ( 'NONE',  ( -1.000000000000000000, 0.000000000000000000, 0.000000000000000000 ) ) ;
#14060 = DIRECTION ( 'NONE',  ( -0.000000000000000000, -0.000000000000000000, -1.000000000000000000 ) ) ;
#14061 = LINE ( 'NONE', #4328, #9576 ) ;
#14062 = VECTOR ( 'NONE', #6920, 1000.000000000000000 ) ;
#14063 = CARTESIAN_POINT ( 'NONE',  ( 5.599999999999994316, -2.020725942163681399, -3.500000000000010214 ) ) ;
#14064 = MECHANICAL_DESIGN_GEOMETRIC_PRESENTATION_REPRESENTATION (  '', ( #12171 ), #5402 ) ;
#14065 = DIRECTION ( 'NONE',  ( 1.892425610156516875E-16, 1.000000000000000000, 0.000000000000000000 ) ) ;
#14066 = PRODUCT_CONTEXT ( 'NONE', #12124, 'mechanical' ) ;
#14067 = FACE_OUTER_BOUND ( 'NONE', #9177, .T. ) ;
#14068 = FACE_OUTER_BOUND ( 'NONE', #3999, .T. ) ;
#14069 = FACE_OUTER_BOUND ( 'NONE', #5480, .T. ) ;
#14070 = EDGE_LOOP ( 'NONE', ( #6646, #12294, #4066, #8663 ) ) ;
#14071 = VECTOR ( 'NONE', #1831, 1000.000000000000000 ) ;
#14072 = VECTOR ( 'NONE', #6879, 1000.000000000000114 ) ;
#14073 = ORIENTED_EDGE ( 'NONE', *, *, #10341, .F. ) ;
#14074 = DIRECTION ( 'NONE',  ( -0.9701425001453319874, -0.2425356250363328026, 0.000000000000000000 ) ) ;
#14075 = LINE ( 'NONE', #9450, #3547 ) ;
#14076 = EDGE_CURVE ( 'NONE', #815, #14008, #2961, .T. ) ;
#14077 = ADVANCED_FACE ( 'NONE', ( #819 ), #3137, .T. ) ;
#14078 = VECTOR ( 'NONE', #9940, 1000.000000000000000 ) ;
#14079 = ORIENTED_EDGE ( 'NONE', *, *, #12264, .T. ) ;
#14080 = VECTOR ( 'NONE', #11423, 1000.000000000000000 ) ;
#14081 = AXIS2_PLACEMENT_3D ( 'NONE', #6056, #2794, #4975 ) ;
#14082 = CARTESIAN_POINT ( 'NONE',  ( 20.00000000000000355, 30.00000000000000711, -25.00000000000000000 ) ) ;
#14083 = FACE_OUTER_BOUND ( 'NONE', #1537, .T. ) ;
#14084 = ORIENTED_EDGE ( 'NONE', *, *, #9141, .F. ) ;
#14085 = FACE_OUTER_BOUND ( 'NONE', #14330, .T. ) ;
#14086 = ORIENTED_EDGE ( 'NONE', *, *, #3468, .F. ) ;
#14087 = EDGE_CURVE ( 'NONE', #11584, #13624, #3980, .T. ) ;
#14088 = UNCERTAINTY_MEASURE_WITH_UNIT (LENGTH_MEASURE( 1.000000000000000082E-05 ), #12155, 'distance_accuracy_value', 'NONE');
#14089 = AXIS2_PLACEMENT_3D ( 'NONE', #11343, #1312, #2948 ) ;
#14090 = TOROIDAL_SURFACE ( 'NONE', #7760, 5.384454397937117776, 0.5155456020628805813 ) ;
#14091 = CARTESIAN_POINT ( 'NONE',  ( 0.000000000000000000, 25.49999999999996803, 0.000000000000000000 ) ) ;
#14092 = DIRECTION ( 'NONE',  ( 0.000000000000000000, -0.4999999999999996114, -0.8660254037844388186 ) ) ;
#14093 = DIRECTION ( 'NONE',  ( 0.000000000000000000, 0.000000000000000000, 1.000000000000000000 ) ) ;
#14094 = ORIENTED_EDGE ( 'NONE', *, *, #4834, .T. ) ;
#14095 = DIRECTION ( 'NONE',  ( 0.000000000000000000, 0.000000000000000000, 1.000000000000000000 ) ) ;
#14096 = FACE_BOUND ( 'NONE', #481, .T. ) ;
#14097 = EDGE_CURVE ( 'NONE', #12770, #13043, #12088, .T. ) ;
#14098 = VERTEX_POINT ( 'NONE', #1998 ) ;
#14099 = SPHERICAL_SURFACE ( 'NONE', #13154, 5.315148208181398104 ) ;
#14100 = ORIENTED_EDGE ( 'NONE', *, *, #3167, .F. ) ;
#14101 = ORIENTED_EDGE ( 'NONE', *, *, #12749, .T. ) ;
#14102 = DIRECTION ( 'NONE',  ( 0.000000000000000000, 0.000000000000000000, -1.000000000000000000 ) ) ;
#14103 = AXIS2_PLACEMENT_3D ( 'NONE', #4498, #1254, #2061 ) ;
#14104 = CIRCLE ( 'NONE', #7770, 5.200000000000001066 ) ;
#14105 = CARTESIAN_POINT ( 'NONE',  ( -3.081487911019577365E-30, 3.469446951953614189E-15, -6.000000000000005329 ) ) ;
#14106 = ORIENTED_EDGE ( 'NONE', *, *, #10521, .F. ) ;
#14107 = CARTESIAN_POINT ( 'NONE',  ( 54.35294117647056567, -1.411764705882362358, 23.00000000000000000 ) ) ;
#14108 = DIRECTION ( 'NONE',  ( 0.000000000000000000, 0.000000000000000000, 1.000000000000000000 ) ) ;
#14109 = ORIENTED_EDGE ( 'NONE', *, *, #13345, .F. ) ;
#14110 = ADVANCED_FACE ( 'NONE', ( #618 ), #12990, .F. ) ;
#14111 = ORIENTED_EDGE ( 'NONE', *, *, #3641, .F. ) ;
#14112 = DIRECTION ( 'NONE',  ( 0.000000000000000000, -8.482162385747133845E-47, 1.000000000000000000 ) ) ;
#14113 = CARTESIAN_POINT ( 'NONE',  ( -3.973244831464914029, 47.44383994248514824, 3.467973375954350068 ) ) ;
#14114 = ORIENTED_EDGE ( 'NONE', *, *, #14435, .F. ) ;
#14115 = CARTESIAN_POINT ( 'NONE',  ( 4.104070371397483541, -4.047367226856751543, 0.000000000000000000 ) ) ;
#14116 = FACE_OUTER_BOUND ( 'NONE', #13115, .T. ) ;
#14117 = ORIENTED_EDGE ( 'NONE', *, *, #7633, .F. ) ;
#14118 = CARTESIAN_POINT ( 'NONE',  ( 3.950250160040158942, -0.7258013381033927569, 3.499999999999992895 ) ) ;
#14119 = EDGE_CURVE ( 'NONE', #2228, #9772, #9604, .T. ) ;
#14120 = FACE_OUTER_BOUND ( 'NONE', #4448, .T. ) ;
#14121 = CARTESIAN_POINT ( 'NONE',  ( 5.000000000000000000, -2.886751345948152192, -0.5999999999999894307 ) ) ;
#14122 = AXIS2_PLACEMENT_3D ( 'NONE', #6301, #3108, #14012 ) ;
#14123 = ORIENTED_EDGE ( 'NONE', *, *, #12976, .T. ) ;
#14124 = EDGE_CURVE ( 'NONE', #13438, #14008, #5283, .T. ) ;
#14125 = EDGE_CURVE ( 'NONE', #10954, #4122, #3361, .T. ) ;
#14126 = VERTEX_POINT ( 'NONE', #9679 ) ;
#14127 = VECTOR ( 'NONE', #14128, 999.9999999999998863 ) ;
#14128 = DIRECTION ( 'NONE',  ( -0.2425356250363330801, 0.9701425001453319874, 0.000000000000000000 ) ) ;
#14129 = ORIENTED_EDGE ( 'NONE', *, *, #9609, .F. ) ;
#14130 = VERTEX_POINT ( 'NONE', #9533 ) ;
#14131 = FACE_OUTER_BOUND ( 'NONE', #10883, .T. ) ;
#14132 = CARTESIAN_POINT ( 'NONE',  ( 5.599999999999994316, 2.020725942163681399, -3.499999999999996003 ) ) ;
#14133 = AXIS2_PLACEMENT_3D ( 'NONE', #9514, #12801, #12728 ) ;
#14134 = CARTESIAN_POINT ( 'NONE',  ( -24.99999999999998934, 199.5765550933606107, -2.000000000000001776 ) ) ;
#14135 = CARTESIAN_POINT ( 'NONE',  ( 108.6817075744280316, 69.57655509336046862, 0.000000000000000000 ) ) ;
#14136 = CARTESIAN_POINT ( 'NONE',  ( -5.253368672218639013, -3.033033817057793957, -4.659491423763650886 ) ) ;
#14137 = PRODUCT_CONTEXT ( 'NONE', #4579, 'mechanical' ) ;
#14138 = DIRECTION ( 'NONE',  ( 0.000000000000000000, 5.551115123125782702E-17, 1.000000000000000000 ) ) ;
#14139 = DIRECTION ( 'NONE',  ( -0.000000000000000000, -0.000000000000000000, -1.000000000000000000 ) ) ;
#14140 = CIRCLE ( 'NONE', #8259, 2.500000000000002220 ) ;
#14141 = ORIENTED_EDGE ( 'NONE', *, *, #13424, .F. ) ;
#14142 = CARTESIAN_POINT ( 'NONE',  ( 20.00000000000000000, 60.00000000000000711, -25.00000000000000000 ) ) ;
#14143 = EDGE_LOOP ( 'NONE', ( #6402, #6161, #13488, #9811 ) ) ;
#14144 = EDGE_CURVE ( 'NONE', #11757, #9480, #8718, .T. ) ;
#14145 = VERTEX_POINT ( 'NONE', #8505 ) ;
#14146 = ORIENTED_EDGE ( 'NONE', *, *, #3180, .F. ) ;
#14147 = DIRECTION ( 'NONE',  ( 0.2425356250363328026, -0.9701425001453319874, -0.000000000000000000 ) ) ;
#14148 = CARTESIAN_POINT ( 'NONE',  ( 30.10000000000000497, 29.99999999999999645, 25.00000000000000000 ) ) ;
#14149 =( NAMED_UNIT ( * ) SI_UNIT ( $, .STERADIAN. ) SOLID_ANGLE_UNIT ( ) );
#14150 = ORIENTED_EDGE ( 'NONE', *, *, #11068, .F. ) ;
#14151 = CARTESIAN_POINT ( 'NONE',  ( 105.6817075744281311, 124.5765550933606107, 25.00000000000000000 ) ) ;
#14152 = CARTESIAN_POINT ( 'NONE',  ( 3.065261730689029740, 7.410293710401357536, 8.000000000000007105 ) ) ;
#14153 = CARTESIAN_POINT ( 'NONE',  ( 25.39999999999999858, 29.99999999999999645, -34.50000000000000000 ) ) ;
#14154 = EDGE_CURVE ( 'NONE', #12126, #2603, #6436, .T. ) ;
#14155 = ADVANCED_FACE ( 'NONE', ( #10907 ), #14292, .T. ) ;
#14156 = DIRECTION ( 'NONE',  ( 1.000000000000000000, 1.665334536937734071E-16, 0.000000000000000000 ) ) ;
#14157 = CARTESIAN_POINT ( 'NONE',  ( 129.3408537872138595, 189.5765550933606107, -75.00000000000001421 ) ) ;
#14158 = PLANE ( 'NONE',  #7853 ) ;
#14159 = ADVANCED_FACE ( 'NONE', ( #7330 ), #12461, .T. ) ;
#14160 = VERTEX_POINT ( 'NONE', #1782 ) ;
#14161 = DIRECTION ( 'NONE',  ( 1.000000000000000000, 0.000000000000000000, 0.000000000000000000 ) ) ;
#14162 = CARTESIAN_POINT ( 'NONE',  ( 4.942458497589258037, 1.621137229507842781, -4.000000000000002665 ) ) ;
#14163 = ORIENTED_EDGE ( 'NONE', *, *, #10431, .T. ) ;
#14164 = CARTESIAN_POINT ( 'NONE',  ( 31.38313257588138683, 143.6985259526510674, -25.00000000000000000 ) ) ;
#14165 = VERTEX_POINT ( 'NONE', #6229 ) ;
#14166 = CARTESIAN_POINT ( 'NONE',  ( -28.00000000000000355, 29.99999999999999645, 8.000000000000007105 ) ) ;
#14167 = ADVANCED_FACE ( 'NONE', ( #14085 ), #10703, .T. ) ;
#14168 = VERTEX_POINT ( 'NONE', #7680 ) ;
#14169 = DIRECTION ( 'NONE',  ( 1.000000000000000000, 1.723842398015259277E-15, -0.000000000000000000 ) ) ;
#14170 = EDGE_CURVE ( 'NONE', #8457, #1777, #3598, .T. ) ;
#14171 = CARTESIAN_POINT ( 'NONE',  ( 1.243833333692737186, -3.900674643482489046, -2.923144239647423426 ) ) ;
#14172 = EDGE_LOOP ( 'NONE', ( #13808, #2497 ) ) ;
#14173 = CARTESIAN_POINT ( 'NONE',  ( 1.560000000000005826, 1.732050807568871864, 0.000000000000000000 ) ) ;
#14174 = CARTESIAN_POINT ( 'NONE',  ( 4.686019787951567928, 9.324138683375338132E-15, 3.999999999999974243 ) ) ;
#14175 = EDGE_CURVE ( 'NONE', #6958, #13484, #6662, .T. ) ;
#14176 = ORIENTED_EDGE ( 'NONE', *, *, #13522, .T. ) ;
#14177 = ORIENTED_EDGE ( 'NONE', *, *, #7642, .T. ) ;
#14178 = CARTESIAN_POINT ( 'NONE',  ( 0.000000000000000000, 40.49999999999999289, 8.000000000000007105 ) ) ;
#14179 = CARTESIAN_POINT ( 'NONE',  ( 24.99999999999999289, -4.898587196589414604E-15, -25.00000000000000000 ) ) ;
#14180 = ORIENTED_EDGE ( 'NONE', *, *, #4661, .F. ) ;
#14181 = DIRECTION ( 'NONE',  ( -1.000000000000000000, 0.000000000000000000, 0.000000000000000000 ) ) ;
#14182 = CARTESIAN_POINT ( 'NONE',  ( 0.000000000000000000, 40.49999999999999289, 0.000000000000000000 ) ) ;
#14183 = EDGE_CURVE ( 'NONE', #11527, #5483, #1482, .T. ) ;
#14184 = CARTESIAN_POINT ( 'NONE',  ( -118.6817075744282306, 109.5765550933602697, 0.000000000000000000 ) ) ;
#14185 = DIRECTION ( 'NONE',  ( -1.000000000000000000, 0.000000000000000000, 0.000000000000000000 ) ) ;
#14186 = VERTEX_POINT ( 'NONE', #3397 ) ;
#14187 = FACE_OUTER_BOUND ( 'NONE', #5487, .T. ) ;
#14188 = EDGE_CURVE ( 'NONE', #10067, #5040, #11526, .T. ) ;
#14189 = DIRECTION ( 'NONE',  ( 0.000000000000000000, 0.000000000000000000, 1.000000000000000000 ) ) ;
#14190 = AXIS2_PLACEMENT_3D ( 'NONE', #2342, #14093, #7177 ) ;
#14191 = ORIENTED_EDGE ( 'NONE', *, *, #75, .F. ) ;
#14192 = CARTESIAN_POINT ( 'NONE',  ( 6.800000000000084199, 4.618802153517023612, -1.387778780781445676E-14 ) ) ;
#14193 = VERTEX_POINT ( 'NONE', #6589 ) ;
#14194 = ORIENTED_EDGE ( 'NONE', *, *, #2836, .F. ) ;
#14195 = DIRECTION ( 'NONE',  ( -3.916739600140467622E-15, 1.000000000000000000, 0.000000000000000000 ) ) ;
#14196 = B_SPLINE_CURVE_WITH_KNOTS ( 'NONE', 3,
 ( #5892, #8023, #9194, #6861, #11323, #1443 ),
 .UNSPECIFIED., .F., .F.,
 ( 4, 2, 4 ),
 ( 0.002336974151641588518, 0.003500975885716462767, 0.004664977619791337016 ),
 .UNSPECIFIED. ) ;
#14197 = DIRECTION ( 'NONE',  ( 1.000000000000000000, 1.224646799147353454E-16, -0.000000000000000000 ) ) ;
#14198 = CARTESIAN_POINT ( 'NONE',  ( 3.868826622783372304, 47.50255440539075380, 2.950282236837604266 ) ) ;
#14199 = PLANE ( 'NONE',  #872 ) ;
#14200 = VECTOR ( 'NONE', #2902, 1000.000000000000114 ) ;
#14201 = CARTESIAN_POINT ( 'NONE',  ( 54.35294117647056567, -1.411764705882362358, 23.00000000000000000 ) ) ;
#14202 = SHAPE_DEFINITION_REPRESENTATION ( #6829, #10940 ) ;
#14203 = CARTESIAN_POINT ( 'NONE',  ( -3.081487911019577365E-30, 3.469446951953614189E-15, -25.03750572909319061 ) ) ;
#14204 = EDGE_CURVE ( 'NONE', #73, #9142, #8856, .T. ) ;
#14205 = DIRECTION ( 'NONE',  ( -1.000000000000000000, 0.000000000000000000, 0.000000000000000000 ) ) ;
#14206 = VECTOR ( 'NONE', #4314, 1000.000000000000000 ) ;
#14207 = ORIENTED_EDGE ( 'NONE', *, *, #13019, .F. ) ;
#14208 = FACE_OUTER_BOUND ( 'NONE', #9052, .T. ) ;
#14209 = ORIENTED_EDGE ( 'NONE', *, *, #5216, .T. ) ;
#14210 = ORIENTED_EDGE ( 'NONE', *, *, #6202, .F. ) ;
#14211 =( REPRESENTATION_RELATIONSHIP ('NONE','NONE', #10295, #4961 ) REPRESENTATION_RELATIONSHIP_WITH_TRANSFORMATION ( #3651 )SHAPE_REPRESENTATION_RELATIONSHIP( ) );
#14212 = ORIENTED_EDGE ( 'NONE', *, *, #784, .F. ) ;
#14213 = VECTOR ( 'NONE', #9175, 1000.000000000000000 ) ;
#14214 = CARTESIAN_POINT ( 'NONE',  ( 22.28098402457126426, 141.4229888148238103, 1.219362754841566419E-12 ) ) ;
#14215 = DIRECTION ( 'NONE',  ( 0.000000000000000000, 0.000000000000000000, 1.000000000000000000 ) ) ;
#14216 = DIRECTION ( 'NONE',  ( -0.000000000000000000, -0.000000000000000000, -1.000000000000000000 ) ) ;
#14217 = EDGE_CURVE ( 'NONE', #3543, #13416, #3323, .T. ) ;
#14218 = ORIENTED_EDGE ( 'NONE', *, *, #13155, .F. ) ;
#14219 = EDGE_CURVE ( 'NONE', #3170, #10977, #1108, .T. ) ;
#14220 = CYLINDRICAL_SURFACE ( 'NONE', #187, 2.500000000000002220 ) ;
#14221 = CONICAL_SURFACE ( 'NONE', #5772, 3.000000000000000888, 0.9599310885968798113 ) ;
#14222 = VECTOR ( 'NONE', #7809, 1000.000000000000000 ) ;
#14223 = CARTESIAN_POINT ( 'NONE',  ( 3.667453972563985829E-15, 6.066067634115573703, -4.659491423763650886 ) ) ;
#14224 = DIRECTION ( 'NONE',  ( 0.000000000000000000, 0.000000000000000000, -1.000000000000000000 ) ) ;
#14225 = UNCERTAINTY_MEASURE_WITH_UNIT (LENGTH_MEASURE( 1.000000000000000082E-05 ), #7572, 'distance_accuracy_value', 'NONE');
#14226 = LINE ( 'NONE', #2000, #13362 ) ;
#14227 = DIRECTION ( 'NONE',  ( 0.000000000000000000, 1.000000000000000000, 0.000000000000000000 ) ) ;
#14228 = LINE ( 'NONE', #10852, #13035 ) ;
#14229 = AXIS2_PLACEMENT_3D ( 'NONE', #6411, #2853, #848 ) ;
#14230 = VECTOR ( 'NONE', #1517, 1000.000000000000000 ) ;
#14231 = LINE ( 'NONE', #10040, #7952 ) ;
#14232 = CARTESIAN_POINT ( 'NONE',  ( 108.6817075744280174, 109.5765550933605113, 1.102182119232617753E-14 ) ) ;
#14233 = AXIS2_PLACEMENT_3D ( 'NONE', #11009, #2992, #2171 ) ;
#14234 = DIRECTION ( 'NONE',  ( -1.000000000000000000, 4.625929269271485914E-16, 0.000000000000000000 ) ) ;
#14235 = ORIENTED_EDGE ( 'NONE', *, *, #1381, .T. ) ;
#14236 = DIRECTION ( 'NONE',  ( -1.000000000000000000, 0.000000000000000000, 0.000000000000000000 ) ) ;
#14237 = CARTESIAN_POINT ( 'NONE',  ( 13.00000000000000533, 35.49999999999997158, 8.000000000000007105 ) ) ;
#14238 = ORIENTED_EDGE ( 'NONE', *, *, #10726, .F. ) ;
#14239 = CARTESIAN_POINT ( 'NONE',  ( 4.988724804725896966, 4.618802153517016507, 1.387778780781445676E-14 ) ) ;
#14240 = DIRECTION ( 'NONE',  ( 1.000000000000000000, 0.000000000000000000, 0.000000000000000000 ) ) ;
#14241 = CIRCLE ( 'NONE', #12819, 3.299999999999969624 ) ;
#14242 = ORIENTED_EDGE ( 'NONE', *, *, #3901, .T. ) ;
#14243 = EDGE_LOOP ( 'NONE', ( #7022, #13976 ) ) ;
#14244 = CARTESIAN_POINT ( 'NONE',  ( 4.198928548860776822, -0.8158838809860106123, -3.226471437616904137 ) ) ;
#14245 = CARTESIAN_POINT ( 'NONE',  ( 5.599999999999994316, 0.000000000000000000, 0.000000000000000000 ) ) ;
#14246 = EDGE_CURVE ( 'NONE', #10176, #2725, #11063, .T. ) ;
#14247 = ORIENTED_EDGE ( 'NONE', *, *, #9141, .T. ) ;
#14248 = CARTESIAN_POINT ( 'NONE',  ( 5.076540720129293582, -2.330508241952930604, 4.036558682520535513 ) ) ;
#14249 = CARTESIAN_POINT ( 'NONE',  ( 20.00000000000000000, 80.00000000000000000, -25.00000000000000000 ) ) ;
#14250 = FACE_OUTER_BOUND ( 'NONE', #10787, .T. ) ;
#14251 = LINE ( 'NONE', #913, #13762 ) ;
#14252 = ORIENTED_EDGE ( 'NONE', *, *, #2745, .F. ) ;
#14253 = CARTESIAN_POINT ( 'NONE',  ( -3.081487911019577365E-30, 3.469446951953614189E-15, -5.624496230895170257 ) ) ;
#14254 = CIRCLE ( 'NONE', #4899, 5.000000000000018652 ) ;
#14255 = EDGE_CURVE ( 'NONE', #6248, #687, #6737, .T. ) ;
#14256 = EDGE_CURVE ( 'NONE', #12252, #3420, #8943, .T. ) ;
#14257 = DIRECTION ( 'NONE',  ( 1.000000000000000000, 0.000000000000000000, 0.000000000000000000 ) ) ;
#14258 = DIRECTION ( 'NONE',  ( 1.000000000000000000, 0.000000000000000000, 0.000000000000000000 ) ) ;
#14259 = ORIENTED_EDGE ( 'NONE', *, *, #12907, .F. ) ;
#14260 = VERTEX_POINT ( 'NONE', #9894 ) ;
#14261 = CONICAL_SURFACE ( 'NONE', #8640, 2.100000000000000977, 1.029744258676656754 ) ;
#14262 = CARTESIAN_POINT ( 'NONE',  ( 51.90514726928103073, 42.68717498692012668, -25.00000000000000000 ) ) ;
#14263 = ADVANCED_FACE ( 'NONE', ( #4353 ), #5498, .F. ) ;
#14264 = EDGE_LOOP ( 'NONE', ( #9009, #10556, #2435, #14259 ) ) ;
#14265 = DIRECTION ( 'NONE',  ( 0.000000000000000000, 0.000000000000000000, 1.000000000000000000 ) ) ;
#14266 = LINE ( 'NONE', #3011, #12587 ) ;
#14267 = CARTESIAN_POINT ( 'NONE',  ( 3.177713737242649827, 47.84352126631787172, 6.443209146269484933 ) ) ;
#14268 = DIRECTION ( 'NONE',  ( -1.000000000000000000, 0.000000000000000000, 0.000000000000000000 ) ) ;
#14269 = DIRECTION ( 'NONE',  ( 1.000000000000000000, 0.000000000000000000, 0.000000000000000000 ) ) ;
#14270 = SHAPE_DEFINITION_REPRESENTATION ( #3823, #852 ) ;
#14271 = CARTESIAN_POINT ( 'NONE',  ( 3.999999999999998224, 2.512222795755935323, -3.169391084040438233 ) ) ;
#14272 = PLANE ( 'NONE',  #3556 ) ;
#14273 = AXIS2_PLACEMENT_3D ( 'NONE', #8973, #6773, #6554 ) ;
#14274 = ORIENTED_EDGE ( 'NONE', *, *, #7422, .T. ) ;
#14275 = CARTESIAN_POINT ( 'NONE',  ( 1.560000000000005826, -0.8660254037844428154, -1.500000000000001332 ) ) ;
#14276 = ORIENTED_EDGE ( 'NONE', *, *, #7534, .F. ) ;
#14277 = ORIENTED_EDGE ( 'NONE', *, *, #10625, .F. ) ;
#14278 = CARTESIAN_POINT ( 'NONE',  ( 22.00000000000000711, 20.00000000000000355, 25.00000000000000000 ) ) ;
#14279 = EDGE_CURVE ( 'NONE', #10817, #4904, #1041, .T. ) ;
#14280 = STYLED_ITEM ( 'NONE', ( #13886 ), #11661 ) ;
#14281 = CONICAL_SURFACE ( 'NONE', #1653, 1732.050807568857181, 1.047197551196592746 ) ;
#14282 = LINE ( 'NONE', #2128, #5659 ) ;
#14283 = CARTESIAN_POINT ( 'NONE',  ( -31.44014396567295577, 21.68342561534834445, 8.000000000000007105 ) ) ;
#14284 = CIRCLE ( 'NONE', #7724, 3.299999999999969624 ) ;
#14285 = DIRECTION ( 'NONE',  ( 0.000000000000000000, 1.000000000000000000, 0.000000000000000000 ) ) ;
#14286 = DIRECTION ( 'NONE',  ( 1.000000000000000000, 0.000000000000000000, 0.000000000000000000 ) ) ;
#14287 = EDGE_CURVE ( 'NONE', #10480, #3697, #334, .T. ) ;
#14288 = VERTEX_POINT ( 'NONE', #9479 ) ;
#14289 = CARTESIAN_POINT ( 'NONE',  ( 39.77836601746437850, 91.19429999418670718, 25.00000000000000000 ) ) ;
#14290 = AXIS2_PLACEMENT_3D ( 'NONE', #2850, #7295, #421 ) ;
#14291 = CARTESIAN_POINT ( 'NONE',  ( 32.42765351673771335, 110.5971499970933536, 25.00000000000000000 ) ) ;
#14292 = PLANE ( 'NONE',  #11514 ) ;
#14293 = CARTESIAN_POINT ( 'NONE',  ( 0.1756478951291663981, -4.720212513052437941, -3.169390900447843329 ) ) ;
#14294 = EDGE_CURVE ( 'NONE', #698, #661, #11588, .T. ) ;
#14295 = PRODUCT_RELATED_PRODUCT_CATEGORY ( 'part', '', ( #12326 ) ) ;
#14296 = EDGE_CURVE ( 'NONE', #10543, #3640, #6379, .T. ) ;
#14297 = CARTESIAN_POINT ( 'NONE',  ( -118.6817075744282306, 109.5765550933602697, -3.299999999999976730 ) ) ;
#14298 = CARTESIAN_POINT ( 'NONE',  ( 6.118061346828462449E-15, -30.42344490663947809, 33.00000000000002842 ) ) ;
#14299 = CARTESIAN_POINT ( 'NONE',  ( 0.000000000000000000, 0.000000000000000000, 0.000000000000000000 ) ) ;
#14300 = VECTOR ( 'NONE', #10453, 1000.000000000000000 ) ;
#14301 = DIRECTION ( 'NONE',  ( -0.5000000000000033307, -0.8660254037844368202, 8.404057939144363410E-32 ) ) ;
#14302 = AXIS2_PLACEMENT_3D ( 'NONE', #5629, #13483, #1250 ) ;
#14303 = CARTESIAN_POINT ( 'NONE',  ( 4.846992820204762076, 0.8286880900430499963, -4.000000000000002665 ) ) ;
#14304 = SHAPE_REPRESENTATION_RELATIONSHIP ( 'NONE' , 'NONE' ,  #4344, #8181 ) ;
#14305 = DIRECTION ( 'NONE',  ( 0.000000000000000000, 0.000000000000000000, -1.000000000000000000 ) ) ;
#14306 = VERTEX_POINT ( 'NONE', #10419 ) ;
#14307 = CARTESIAN_POINT ( 'NONE',  ( -5.384454397937117776, -2.411715596982285058E-16, -4.699999999999981526 ) ) ;
#14308 = FACE_OUTER_BOUND ( 'NONE', #12435, .T. ) ;
#14309 = ORIENTED_EDGE ( 'NONE', *, *, #5526, .F. ) ;
#14310 = LINE ( 'NONE', #7557, #6461 ) ;
#14311 = VECTOR ( 'NONE', #6188, 1000.000000000000000 ) ;
#14312 = CARTESIAN_POINT ( 'NONE',  ( 22.28098402457051463, 141.4229888148235830, -32.99999999999999289 ) ) ;
#14313 = VECTOR ( 'NONE', #5995, 1000.000000000000000 ) ;
#14314 = AXIS2_PLACEMENT_3D ( 'NONE', #4079, #969, #8518 ) ;
#14315 = VERTEX_POINT ( 'NONE', #9322 ) ;
#14316 = EDGE_CURVE ( 'NONE', #1016, #4305, #3924, .T. ) ;
#14317 = EDGE_LOOP ( 'NONE', ( #13340, #7551, #5616, #11263 ) ) ;
#14318 = CARTESIAN_POINT ( 'NONE',  ( -140.0000000000003411, 189.5765550933606107, 47.99999999999998579 ) ) ;
#14319 = CARTESIAN_POINT ( 'NONE',  ( 36.99999999999999289, 80.00000000000000000, 25.00000000000000000 ) ) ;
#14320 = ORIENTED_EDGE ( 'NONE', *, *, #8337, .F. ) ;
#14321 = CARTESIAN_POINT ( 'NONE',  ( 108.6817075744280174, 39.57655509336063915, -117.0000000000000000 ) ) ;
#14322 = DIRECTION ( 'NONE',  ( -1.224646799147353454E-16, 1.000000000000000000, 0.000000000000000000 ) ) ;
#14323 = ADVANCED_BREP_SHAPE_REPRESENTATION ( '', ( #6797, #11025 ), #532 ) ;
#14324 = DIRECTION ( 'NONE',  ( -0.2425356250363328026, 0.9701425001453319874, 0.000000000000000000 ) ) ;
#14325 = CARTESIAN_POINT ( 'NONE',  ( -4.319324222799853175, 3.279739689145492854, -4.138711833384279615 ) ) ;
#14326 = VECTOR ( 'NONE', #12889, 1000.000000000000000 ) ;
#14327 = ORIENTED_EDGE ( 'NONE', *, *, #12907, .T. ) ;
#14328 = DIRECTION ( 'NONE',  ( -1.000000000000000000, 0.000000000000000000, 0.000000000000000000 ) ) ;
#14329 = DIRECTION ( 'NONE',  ( 1.734723475976770502E-18, -4.440892098500621231E-16, -1.000000000000000000 ) ) ;
#14330 = EDGE_LOOP ( 'NONE', ( #13652, #10252, #13648, #7664 ) ) ;
#14331 =( BOUNDED_SURFACE ( )  B_SPLINE_SURFACE ( 3, 2, ( 
 ( #3838, #8270, #7538 ),
 ( #4135, #13929, #6376 ),
 ( #12905, #686, #8502 ),
 ( #7328, #7246, #3902 ),
 ( #11872, #10700, #2888 ),
 ( #12826, #11726, #11803 ) ),
 .UNSPECIFIED., .F., .F., .T. ) 
 B_SPLINE_SURFACE_WITH_KNOTS ( ( 4, 2, 4 ),
 ( 3, 3 ),
 ( 0.002450104044831692002, 0.005591829551853677756, 0.008733555058875663510 ),
 ( 0.000000000000000000, 1.000000000000000000 ),
 .UNSPECIFIED. ) 
 GEOMETRIC_REPRESENTATION_ITEM ( )  RATIONAL_B_SPLINE_SURFACE ( (
 ( 1.000000000000000000, 0.8047731410850404998, 1.000000000000000000),
 ( 1.000000000000000000, 0.8125552299158004255, 1.000000000000000000),
 ( 1.000000000000000000, 0.8191520442887517683, 1.000000000000000000),
 ( 1.000000000000000000, 0.8191520442892222809, 1.000000000000000000),
 ( 1.000000000000000000, 0.8125552299154461533, 1.000000000000000000),
 ( 1.000000000000000000, 0.8047731410850398337, 1.000000000000000000) ) ) 
 REPRESENTATION_ITEM ( '' )  SURFACE ( )  );
#14332 = CIRCLE ( 'NONE', #7314, 2.500000000000002220 ) ;
#14333 = ORIENTED_EDGE ( 'NONE', *, *, #8159, .T. ) ;
#14334 = ADVANCED_FACE ( 'NONE', ( #12608 ), #13806, .T. ) ;
#14335 = CARTESIAN_POINT ( 'NONE',  ( 1.560000000000005826, -1.299038105676650456, -0.7500000000000006661 ) ) ;
#14336 = EDGE_LOOP ( 'NONE', ( #6015, #10051, #13742, #13945 ) ) ;
#14337 = CARTESIAN_POINT ( 'NONE',  ( 108.6817075744280601, 39.57655509336063915, -106.9999999999999858 ) ) ;
#14338 = FACE_OUTER_BOUND ( 'NONE', #2911, .T. ) ;
#14339 = CARTESIAN_POINT ( 'NONE',  ( 2.650472254991407706, 48.05066328782152141, 7.006789553262801284 ) ) ;
#14340 = DIRECTION ( 'NONE',  ( 0.000000000000000000, 0.000000000000000000, -1.000000000000000000 ) ) ;
#14341 = ADVANCED_FACE ( 'NONE', ( #2830 ), #12956, .F. ) ;
#14342 = CARTESIAN_POINT ( 'NONE',  ( 44.62907851819101523, 71.79144999128007498, -25.00000000000000000 ) ) ;
#14343 = APPLICATION_PROTOCOL_DEFINITION ( 'draft international standard', 'automotive_design', 1998, #7067 ) ;
#14344 = EDGE_CURVE ( 'NONE', #2567, #12697, #4757, .T. ) ;
#14345 = LINE ( 'NONE', #12285, #8421 ) ;
#14346 = CARTESIAN_POINT ( 'NONE',  ( 4.170895651974821483, 2.054890354522617812, -3.559174498016382859 ) ) ;
#14347 = ORIENTED_EDGE ( 'NONE', *, *, #14287, .T. ) ;
#14348 = ADVANCED_FACE ( 'NONE', ( #259 ), #9248, .T. ) ;
#14349 = DIRECTION ( 'NONE',  ( 1.000000000000000000, 1.665334536937734071E-16, 0.000000000000000000 ) ) ;
#14350 = B_SPLINE_CURVE_WITH_KNOTS ( 'NONE', 3,
 ( #2120, #6495, #3299, #1017, #11040 ),
 .UNSPECIFIED., .F., .F.,
 ( 4, 1, 4 ),
 ( 0.000000000000000000, 0.002309401076758504055, 0.004618802153517008978 ),
 .UNSPECIFIED. ) ;
#14351 = CIRCLE ( 'NONE', #5457, 2.600000000000004974 ) ;
#14352 = ORIENTED_EDGE ( 'NONE', *, *, #6443, .T. ) ;
#14353 = ADVANCED_FACE ( 'NONE', ( #12764 ), #9925, .F. ) ;
#14354 = ORIENTED_EDGE ( 'NONE', *, *, #10042, .F. ) ;
#14355 = PRODUCT_DEFINITION_FORMATION_WITH_SPECIFIED_SOURCE ( 'ANY', '', #63, .NOT_KNOWN. ) ;
#14356 = DIRECTION ( 'NONE',  ( 0.000000000000000000, 0.000000000000000000, 1.000000000000000000 ) ) ;
#14357 =( NAMED_UNIT ( * ) SI_UNIT ( $, .STERADIAN. ) SOLID_ANGLE_UNIT ( ) );
#14358 = DIRECTION ( 'NONE',  ( 0.000000000000000000, 0.000000000000000000, 1.000000000000000000 ) ) ;
#14359 = CARTESIAN_POINT ( 'NONE',  ( 5.085009042717541838, 4.657032265668563653, 0.06621649662554610072 ) ) ;
#14360 = DIRECTION ( 'NONE',  ( 1.000000000000000000, 0.000000000000000000, 0.000000000000000000 ) ) ;
#14361 = VECTOR ( 'NONE', #13657, 1000.000000000000000 ) ;
#14362 = B_SPLINE_CURVE_WITH_KNOTS ( 'NONE', 3,
 ( #2781, #4027, #1591, #1524, #8170, #9503 ),
 .UNSPECIFIED., .F., .F.,
 ( 4, 2, 4 ),
 ( 0.000000000000000000, 0.0002095117440854733651, 0.0004190234881709467302 ),
 .UNSPECIFIED. ) ;
#14363 = ORIENTED_EDGE ( 'NONE', *, *, #8734, .F. ) ;
#14364 = ORIENTED_EDGE ( 'NONE', *, *, #150, .F. ) ;
#14365 = DIRECTION ( 'NONE',  ( 0.000000000000000000, 0.000000000000000000, -1.000000000000000000 ) ) ;
#14366 = EDGE_CURVE ( 'NONE', #12770, #1645, #560, .T. ) ;
#14367 = CARTESIAN_POINT ( 'NONE',  ( -1.752700365193367750E-15, -5.773502691896304384, -4.284345921091780696 ) ) ;
#14368 = CARTESIAN_POINT ( 'NONE',  ( 76.68170757442801744, 29.57655509336063204, 33.00000000000000000 ) ) ;
#14369 = EDGE_LOOP ( 'NONE', ( #567, #6758, #289, #9123 ) ) ;
#14370 = CARTESIAN_POINT ( 'NONE',  ( 108.6817075744280459, 109.5765550933604828, 3.299999999999976730 ) ) ;
#14371 = PRODUCT_DEFINITION_CONTEXT ( 'detailed design', #552, 'design' ) ;
#14372 = DIRECTION ( 'NONE',  ( -1.000000000000000000, -8.619211990076296383E-16, 1.276920294826117846E-16 ) ) ;
#14373 = CARTESIAN_POINT ( 'NONE',  ( 62.10586122665986863, -20.42344490663941414, -27.99999999999999645 ) ) ;
#14374 = CARTESIAN_POINT ( 'NONE',  ( 20.00000000000000355, 30.00000000000000711, 25.00000000000000000 ) ) ;
#14375 = DIRECTION ( 'NONE',  ( 0.8660254037844367092, -0.5000000000000032196, 2.348866325434811866E-33 ) ) ;
#14376 = CARTESIAN_POINT ( 'NONE',  ( 0.000000000000000000, 0.000000000000000000, 0.000000000000000000 ) ) ;
#14377 = B_SPLINE_CURVE_WITH_KNOTS ( 'NONE', 3,
 ( #2550, #11538, #6039, #282, #4748, #9195 ),
 .UNSPECIFIED., .F., .F.,
 ( 4, 2, 4 ),
 ( 0.004308305454211655387, 0.005784651566377436299, 0.007260997678543217211 ),
 .UNSPECIFIED. ) ;
#14378 = FILL_AREA_STYLE_COLOUR ( '', #9410 ) ;
#14379 = LINE ( 'NONE', #1939, #11734 ) ;
#14380 = ORIENTED_EDGE ( 'NONE', *, *, #4547, .F. ) ;
#14381 = APPLICATION_CONTEXT ( 'automotive_design' ) ;
#14382 = CARTESIAN_POINT ( 'NONE',  ( 5.000000000000000000, -2.886751345948148639, -4.284345921091780696 ) ) ;
#14383 = EDGE_CURVE ( 'NONE', #1326, #7871, #11518, .T. ) ;
#14384 = VERTEX_POINT ( 'NONE', #1421 ) ;
#14385 = DIRECTION ( 'NONE',  ( 0.000000000000000000, 1.000000000000000000, 0.000000000000000000 ) ) ;
#14386 = CARTESIAN_POINT ( 'NONE',  ( 31.24550000000003536, 0.000000000000000000, 0.000000000000000000 ) ) ;
#14387 = ORIENTED_EDGE ( 'NONE', *, *, #241, .T. ) ;
#14388 = ORIENTED_EDGE ( 'NONE', *, *, #3124, .T. ) ;
#14389 = CARTESIAN_POINT ( 'NONE',  ( 4.204015924366194312, -1.626724848190931771, -3.310627190413377274 ) ) ;
#14390 = CARTESIAN_POINT ( 'NONE',  ( -3.500188911486803889, -4.028306647601596069, -4.385926550512758482 ) ) ;
#14391 = CIRCLE ( 'NONE', #827, 8.000000000000000000 ) ;
#14392 = DIRECTION ( 'NONE',  ( 0.000000000000000000, 1.000000000000000000, 0.000000000000000000 ) ) ;
#14393 = FACE_OUTER_BOUND ( 'NONE', #2645, .T. ) ;
#14394 = DIRECTION ( 'NONE',  ( 1.000000000000000000, 1.723842398015259277E-15, 0.000000000000000000 ) ) ;
#14395 = CARTESIAN_POINT ( 'NONE',  ( -3.401922400371467425, 3.809401878279565334, -4.271474537231044977 ) ) ;
#14396 = ORIENTED_EDGE ( 'NONE', *, *, #12749, .F. ) ;
#14397 = DIRECTION ( 'NONE',  ( -1.000000000000000000, 0.000000000000000000, 0.000000000000000000 ) ) ;
#14398 = DIRECTION ( 'NONE',  ( 0.000000000000000000, 0.000000000000000000, -1.000000000000000000 ) ) ;
#14399 = EDGE_CURVE ( 'NONE', #2703, #8390, #12926, .T. ) ;
#14400 = EDGE_CURVE ( 'NONE', #13250, #4441, #1798, .T. ) ;
#14401 = FACE_OUTER_BOUND ( 'NONE', #9664, .T. ) ;
#14402 = AXIS2_PLACEMENT_3D ( 'NONE', #11135, #6740, #4503 ) ;
#14403 = ORIENTED_EDGE ( 'NONE', *, *, #10724, .F. ) ;
#14404 = ORIENTED_EDGE ( 'NONE', *, *, #5542, .F. ) ;
#14405 = ORIENTED_EDGE ( 'NONE', *, *, #1057, .T. ) ;
#14406 = CARTESIAN_POINT ( 'NONE',  ( -140.0000000000003411, 199.5765550933606107, 47.99999999999998579 ) ) ;
#14407 = ORIENTED_EDGE ( 'NONE', *, *, #4847, .T. ) ;
#14408 = LINE ( 'NONE', #3502, #4678 ) ;
#14409 = CARTESIAN_POINT ( 'NONE',  ( 31.44014396567294867, 38.31657438465161647, 0.000000000000000000 ) ) ;
#14410 = PLANE ( 'NONE',  #10746 ) ;
#14411 = FACE_OUTER_BOUND ( 'NONE', #13944, .T. ) ;
#14412 = DIRECTION ( 'NONE',  ( -1.000000000000000000, 2.551526159633733968E-19, 1.987661601597216239E-18 ) ) ;
#14413 = CARTESIAN_POINT ( 'NONE',  ( 19.99999999999999645, 67.00000000000000000, -25.00000000000000000 ) ) ;
#14414 = CARTESIAN_POINT ( 'NONE',  ( 5.046772446839293380, -4.635550663945605443, -1.375445609632852674E-14 ) ) ;
#14415 = ADVANCED_FACE ( 'NONE', ( #14308 ), #6247, .F. ) ;
#14416 = ADVANCED_FACE ( 'NONE', ( #4085 ), #11898, .T. ) ;
#14417 = EDGE_LOOP ( 'NONE', ( #10483, #10164, #7863, #8729, #7640, #3147, #3593, #6605, #3410, #4110, #6583, #851, #11115, #4161, #9350, #6586, #8947, #7675, #9137, #7864, #13673, #6284, #12021, #12057, #4924, #1764, #1347, #5726, #2526, #5986 ) ) ;
#14418 = DIRECTION ( 'NONE',  ( 1.000000000000000000, 0.000000000000000000, 0.000000000000000000 ) ) ;
#14419 = VERTEX_POINT ( 'NONE', #9620 ) ;
#14420 = ORIENTED_EDGE ( 'NONE', *, *, #1101, .T. ) ;
#14421 = ORIENTED_EDGE ( 'NONE', *, *, #11822, .F. ) ;
#14422 = LINE ( 'NONE', #11264, #12364 ) ;
#14423 = CIRCLE ( 'NONE', #8088, 0.5499999999999992673 ) ;
#14424 = CARTESIAN_POINT ( 'NONE',  ( -5.000000000000000888, 0.000000000000000000, 0.000000000000000000 ) ) ;
#14425 = LINE ( 'NONE', #2129, #3745 ) ;
#14426 = EDGE_CURVE ( 'NONE', #13171, #6636, #13149, .T. ) ;
#14427 = DIRECTION ( 'NONE',  ( -1.000000000000000000, 0.000000000000000000, 0.000000000000000000 ) ) ;
#14428 = ORIENTED_EDGE ( 'NONE', *, *, #8544, .F. ) ;
#14429 = DIRECTION ( 'NONE',  ( -0.000000000000000000, 0.000000000000000000, 1.000000000000000000 ) ) ;
#14430 = CARTESIAN_POINT ( 'NONE',  ( 22.00000000000000355, 40.00000000000000711, -25.00000000000000000 ) ) ;
#14431 = CYLINDRICAL_SURFACE ( 'NONE', #511, 2.100000000000000977 ) ;
#14432 = AXIS2_PLACEMENT_3D ( 'NONE', #7837, #6515, #13206 ) ;
#14433 = ORIENTED_EDGE ( 'NONE', *, *, #4070, .F. ) ;
#14434 = EDGE_CURVE ( 'NONE', #13539, #192, #13618, .T. ) ;
#14435 = EDGE_CURVE ( 'NONE', #14145, #4441, #8523, .T. ) ;
#14436 = CARTESIAN_POINT ( 'NONE',  ( -108.6817075744282448, 109.5765550933602839, 0.000000000000000000 ) ) ;
#14437 = DIRECTION ( 'NONE',  ( -0.7071067811865513475, 8.659560562354886020E-17, -0.7071067811865436870 ) ) ;
#14438 = CARTESIAN_POINT ( 'NONE',  ( 27.30499999999998195, 0.000000000000000000, 0.000000000000000000 ) ) ;
#14439 = AXIS2_PLACEMENT_3D ( 'NONE', #12121, #2101, #1144 ) ;
#14440 = DIRECTION ( 'NONE',  ( -0.000000000000000000, -1.000000000000000000, 0.000000000000000000 ) ) ;
#14441 = LINE ( 'NONE', #13493, #2250 ) ;
#14442 = CARTESIAN_POINT ( 'NONE',  ( -28.00000000000000355, 29.99999999999999645, 0.000000000000000000 ) ) ;
#14443 = EDGE_CURVE ( 'NONE', #721, #7705, #11969, .T. ) ;
#14444 = CARTESIAN_POINT ( 'NONE',  ( 58.68170757442803165, 29.57655509336062849, 33.00000000000000000 ) ) ;
#14445 = CONICAL_SURFACE ( 'NONE', #11161, 3.499999999999999112, 1.047197551196600296 ) ;
#14446 = CARTESIAN_POINT ( 'NONE',  ( 5.067058822021063058, 2.325541950156907234, 4.027956812804561082 ) ) ;
#14447 = CIRCLE ( 'NONE', #8592, 1.500000000000000000 ) ;
#14448 = ORIENTED_EDGE ( 'NONE', *, *, #2768, .T. ) ;
#14449 = EDGE_LOOP ( 'NONE', ( #692, #12084 ) ) ;
#14450 = DIRECTION ( 'NONE',  ( 0.000000000000000000, 4.440892098500621231E-16, 1.000000000000000000 ) ) ;
#14451 = VERTEX_POINT ( 'NONE', #636 ) ;
#14452 = CARTESIAN_POINT ( 'NONE',  ( 0.000000000000000000, 0.000000000000000000, 0.000000000000000000 ) ) ;
#14453 = CARTESIAN_POINT ( 'NONE',  ( 54.35294117647056567, -1.411764705882362358, -23.00000000000000000 ) ) ;
#14454 = AXIS2_PLACEMENT_3D ( 'NONE', #235, #4580, #5776 ) ;
#14455 = AXIS2_PLACEMENT_3D ( 'NONE', #2544, #13684, #12352 ) ;
#14456 = LINE ( 'NONE', #5518, #7555 ) ;
#14457 = CARTESIAN_POINT ( 'NONE',  ( 129.3408537872138595, 199.5765550933606107, -4.000000000000019540 ) ) ;
#14458 = EDGE_CURVE ( 'NONE', #6929, #11189, #9554, .T. ) ;
#14459 = CARTESIAN_POINT ( 'NONE',  ( -129.3408537872145132, 189.5765550933606107, -4.000000000000031086 ) ) ;
#14460 = DIRECTION ( 'NONE',  ( 0.000000000000000000, 0.000000000000000000, 1.000000000000000000 ) ) ;
#14461 = CARTESIAN_POINT ( 'NONE',  ( 20.00000000000000000, 80.00000000000000000, -25.00000000000000000 ) ) ;
#14462 = CARTESIAN_POINT ( 'NONE',  ( 4.175813232069169878, 2.061359961916364725, -3.570380186727395433 ) ) ;
#14463 = EDGE_LOOP ( 'NONE', ( #6066, #13327, #5213, #2389 ) ) ;
#14464 = ORIENTED_EDGE ( 'NONE', *, *, #5819, .T. ) ;
#14465 = NEXT_ASSEMBLY_USAGE_OCCURRENCE ( 'NAUO1', ' ', ' ', #12140, #9274, $ ) ;
#14466 = NEXT_ASSEMBLY_USAGE_OCCURRENCE ( 'NAUO2', ' ', ' ', #12140, #9731, $ ) ;
#14467 = NEXT_ASSEMBLY_USAGE_OCCURRENCE ( 'NAUO3', ' ', ' ', #12140, #12500, $ ) ;
#14468 = NEXT_ASSEMBLY_USAGE_OCCURRENCE ( 'NAUO4', ' ', ' ', #12140, #6941, $ ) ;
#14469 = NEXT_ASSEMBLY_USAGE_OCCURRENCE ( 'NAUO5', ' ', ' ', #12140, #11417, $ ) ;
#14470 = NEXT_ASSEMBLY_USAGE_OCCURRENCE ( 'NAUO6', ' ', ' ', #12140, #7761, $ ) ;
#14471 = NEXT_ASSEMBLY_USAGE_OCCURRENCE ( 'NAUO7', ' ', ' ', #12140, #7761, $ ) ;
#14472 = NEXT_ASSEMBLY_USAGE_OCCURRENCE ( 'NAUO8', ' ', ' ', #12140, #11417, $ ) ;
#14473 = NEXT_ASSEMBLY_USAGE_OCCURRENCE ( 'NAUO9', ' ', ' ', #12140, #12500, $ ) ;
#14474 = NEXT_ASSEMBLY_USAGE_OCCURRENCE ( 'NAUO10', ' ', ' ', #12140, #13230, $ ) ;
#14475 = NEXT_ASSEMBLY_USAGE_OCCURRENCE ( 'NAUO11', ' ', ' ', #12140, #9731, $ ) ;
#14476 = NEXT_ASSEMBLY_USAGE_OCCURRENCE ( 'NAUO12', ' ', ' ', #12140, #7761, $ ) ;
#14477 = NEXT_ASSEMBLY_USAGE_OCCURRENCE ( 'NAUO13', ' ', ' ', #12140, #7761, $ ) ;
#14478 = NEXT_ASSEMBLY_USAGE_OCCURRENCE ( 'NAUO14', ' ', ' ', #12140, #4990, $ ) ;
#14479 = NEXT_ASSEMBLY_USAGE_OCCURRENCE ( 'NAUO15', ' ', ' ', #12140, #3656, $ ) ;
#14480 = NEXT_ASSEMBLY_USAGE_OCCURRENCE ( 'NAUO16', ' ', ' ', #12140, #11244, $ ) ;
#14481 = NEXT_ASSEMBLY_USAGE_OCCURRENCE ( 'NAUO17', ' ', ' ', #12140, #11244, $ ) ;
#14482 = NEXT_ASSEMBLY_USAGE_OCCURRENCE ( 'NAUO18', ' ', ' ', #12140, #13858, $ ) ;
#14483 = NEXT_ASSEMBLY_USAGE_OCCURRENCE ( 'NAUO19', ' ', ' ', #12140, #13858, $ ) ;
#14484 = NEXT_ASSEMBLY_USAGE_OCCURRENCE ( 'NAUO20', ' ', ' ', #12140, #11881, $ ) ;
#14485 = NEXT_ASSEMBLY_USAGE_OCCURRENCE ( 'NAUO21', ' ', ' ', #12140, #11881, $ ) ;
#14486 = NEXT_ASSEMBLY_USAGE_OCCURRENCE ( 'NAUO22', ' ', ' ', #12140, #2574, $ ) ;
#14487 = NEXT_ASSEMBLY_USAGE_OCCURRENCE ( 'NAUO23', ' ', ' ', #12140, #2574, $ ) ;
#14488 = NEXT_ASSEMBLY_USAGE_OCCURRENCE ( 'NAUO24', ' ', ' ', #12140, #2574, $ ) ;
#14489 = NEXT_ASSEMBLY_USAGE_OCCURRENCE ( 'NAUO25', ' ', ' ', #12140, #2574, $ ) ;
#14490 = NEXT_ASSEMBLY_USAGE_OCCURRENCE ( 'NAUO26', ' ', ' ', #12140, #8013, $ ) ;
#14491 = NEXT_ASSEMBLY_USAGE_OCCURRENCE ( 'NAUO27', ' ', ' ', #12140, #8013, $ ) ;
ENDSEC;
END-ISO-10303-21;
